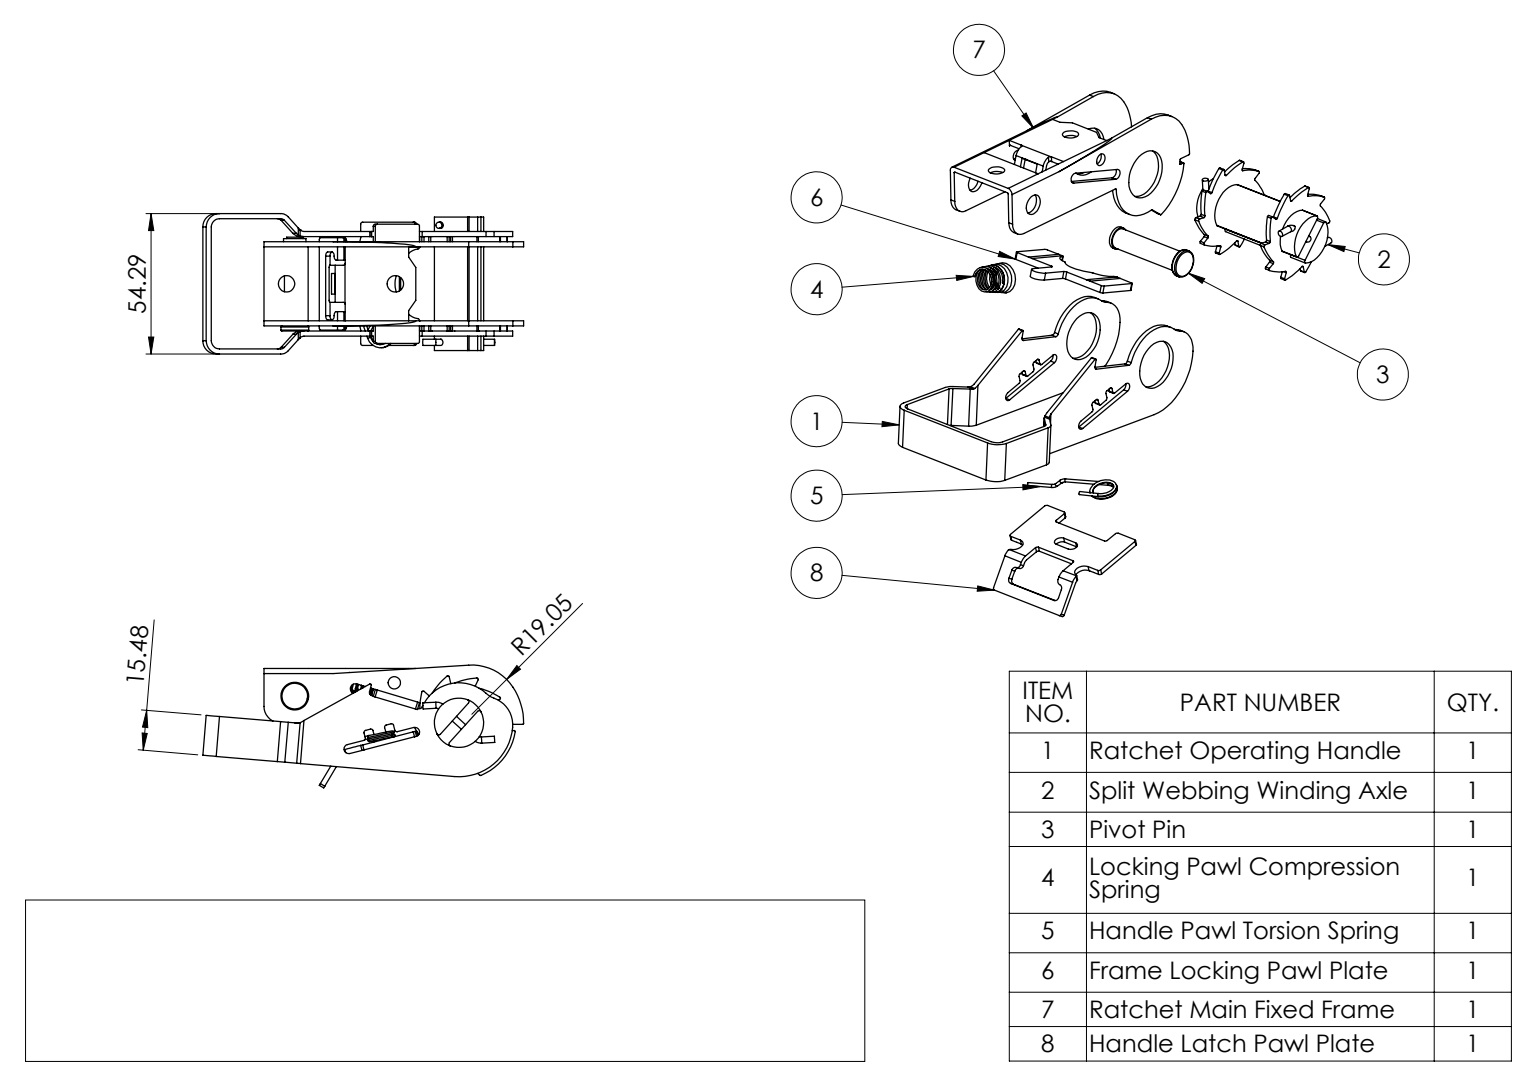
ISO-10303-21;
HEADER;
FILE_DESCRIPTION (('STEP AP214'),
    '1' );
FILE_NAME ('MAS-676',
    '2026-10-09T14:10:49',
    ( '' ),
    ( '' ),
    'SwSTEP 2.0',
    'SolidWorks 2026',
    '' );
FILE_SCHEMA (( 'AUTOMOTIVE_DESIGN' ));
ENDSEC;

DATA;
#1 = VERTEX_POINT ( 'NONE', #18707 ) ;
#2 = CARTESIAN_POINT ( 'NONE',  ( 12.17369753589567871, 10.51393144722840134, 2.800165564711390775 ) ) ;
#3 = CIRCLE ( 'NONE', #8469, 0.5080000000000013394 ) ;
#4 = CARTESIAN_POINT ( 'NONE',  ( 11.85962738539019945, 21.73984789707424170, 3.515838200515787548 ) ) ;
#5 = ORIENTED_EDGE ( 'NONE', *, *, #9450, .F. ) ;
#6 = CARTESIAN_POINT ( 'NONE',  ( 8.350682983910802548, 10.74290543192399028, 2.522985661756687037 ) ) ;
#7 = CARTESIAN_POINT ( 'NONE',  ( 2.865713946637347131, 12.03281576442448042, 5.073952485450168304 ) ) ;
#8 = CARTESIAN_POINT ( 'NONE',  ( -23.01875000000000071, 1.984375000000000000, -3.968750000000000000 ) ) ;
#9 = ADVANCED_FACE ( 'NONE', ( #16944, #16633 ), #1476, .F. ) ;
#10 = CARTESIAN_POINT ( 'NONE',  ( 24.26606285357373594, 2.770822500000000854, -16.92219937337620195 ) ) ;
#11 = CARTESIAN_POINT ( 'NONE',  ( 11.51539948528376733, 12.31998346384714083, 5.480917910381482017 ) ) ;
#12 = VECTOR ( 'NONE', #9469, 1000.000000000000227 ) ;
#13 = VECTOR ( 'NONE', #12201, 1000.000000000000000 ) ;
#14 = CARTESIAN_POINT ( 'NONE',  ( 3.657427262928014677, 14.72322116853433194, 9.063302901626695274 ) ) ;
#15 = CARTESIAN_POINT ( 'NONE',  ( -17.46249999999999858, 1.984375000000000000, 0.000000000000000000 ) ) ;
#16 = CARTESIAN_POINT ( 'NONE',  ( 20.19277141636333894, -1.028702071915735816, -14.77014087419847499 ) ) ;
#17 = CARTESIAN_POINT ( 'NONE',  ( 2.809774020526558225, 19.21875272216368202, 7.448689460942592433 ) ) ;
#18 = CARTESIAN_POINT ( 'NONE',  ( 49.81956284419040060, 0.000000000000000000, 11.98436472153758103 ) ) ;
#19 = CARTESIAN_POINT ( 'NONE',  ( 10.74587282237300023, -3.551474423027108696, -17.13904648846254730 ) ) ;
#20 = STYLED_ITEM ( 'NONE', ( #9424 ), #6575 ) ;
#21 = PLANE ( 'NONE',  #4977 ) ;
#22 = VECTOR ( 'NONE', #6155, 999.9999999999998863 ) ;
#23 = ORIENTED_EDGE ( 'NONE', *, *, #18650, .T. ) ;
#24 = CYLINDRICAL_SURFACE ( 'NONE', #13892, 30.16250000000000142 ) ;
#25 = CARTESIAN_POINT ( 'NONE',  ( 10.71174415246057698, 20.20840087037584709, 6.087647022013951137 ) ) ;
#26 = EDGE_CURVE ( 'NONE', #12400, #1617, #15318, .T. ) ;
#27 = ORIENTED_EDGE ( 'NONE', *, *, #3397, .F. ) ;
#28 = CARTESIAN_POINT ( 'NONE',  ( 12.58269666770059381, 11.55388254762453215, 3.248295542190139606 ) ) ;
#29 = CARTESIAN_POINT ( 'NONE',  ( 53.08681243026497043, 37.69777154208443193, -16.72443647847455850 ) ) ;
#30 = CARTESIAN_POINT ( 'NONE',  ( 16.87573345534896063, 1.342421174834532049, -14.70424319714138583 ) ) ;
#31 = CARTESIAN_POINT ( 'NONE',  ( 6.789087559929837923, 18.21544151669790068, 7.520383359049297667 ) ) ;
#32 = ORIENTED_EDGE ( 'NONE', *, *, #21036, .F. ) ;
#33 = SHAPE_REPRESENTATION_RELATIONSHIP ( 'NONE' , 'NONE' ,  #560, #17207 ) ;
#34 = DIRECTION ( 'NONE',  ( 0.9943660382494290406, 0.000000000000000000, -0.1060008583745199739 ) ) ;
#35 = CARTESIAN_POINT ( 'NONE',  ( -29.36874999999999858, 2.380615000000000148, 8.335010000000000474 ) ) ;
#36 = EDGE_CURVE ( 'NONE', #1582, #17060, #15097, .T. ) ;
#37 = EDGE_CURVE ( 'NONE', #10557, #1153, #11768, .T. ) ;
#38 = ADVANCED_FACE ( 'NONE', ( #13541 ), #20247, .T. ) ;
#39 = CARTESIAN_POINT ( 'NONE',  ( -0.5435003404963313356, 2.373947500000000765, -25.80650133522849998 ) ) ;
#40 = CLOSED_SHELL ( 'NONE', ( #13341, #4807, #5036, #2626, #8435, #8593, #10298, #38, #14436, #19908, #617, #19403, #13246, #15792, #17350, #9101 ) ) ;
#41 = ORIENTED_EDGE ( 'NONE', *, *, #3166, .F. ) ;
#42 = CARTESIAN_POINT ( 'NONE',  ( 9.280550395262261887, 14.88029421051436429, 7.112226467325535317 ) ) ;
#43 = CARTESIAN_POINT ( 'NONE',  ( 11.94459739279681543, 20.94853845629116051, 3.647987758710024675 ) ) ;
#44 = CARTESIAN_POINT ( 'NONE',  ( 3.622293142213341088, 12.24591714145684129, 6.558976304062217544 ) ) ;
#45 = CARTESIAN_POINT ( 'NONE',  ( 6.749462305694075681, 11.05277248166000170, 4.479057920628951805 ) ) ;
#46 = CIRCLE ( 'NONE', #17730, 1.984374999999999112 ) ;
#47 = CARTESIAN_POINT ( 'NONE',  ( 12.03790632155779505, -1.842118199788904453, -16.73074338374886594 ) ) ;
#48 = DIRECTION ( 'NONE',  ( 0.000000000000000000, -1.000000000000000000, 0.000000000000000000 ) ) ;
#49 = ORIENTED_EDGE ( 'NONE', *, *, #10493, .T. ) ;
#50 = CARTESIAN_POINT ( 'NONE',  ( 10.56693948759176571, 19.61111237035978050, 5.589555579635868021 ) ) ;
#51 = CARTESIAN_POINT ( 'NONE',  ( 8.239716553926831111, 21.32987559984598391, 5.052740338774581730 ) ) ;
#52 = EDGE_CURVE ( 'NONE', #9108, #5857, #17721, .T. ) ;
#53 = CARTESIAN_POINT ( 'NONE',  ( 55.27198911326564001, 34.52875999999999834, 2.462719476673013830 ) ) ;
#54 = VECTOR ( 'NONE', #11480, 1000.000000000000000 ) ;
#55 = ORIENTED_EDGE ( 'NONE', *, *, #21504, .F. ) ;
#56 = ORIENTED_EDGE ( 'NONE', *, *, #17494, .T. ) ;
#57 = VECTOR ( 'NONE', #329, 1000.000000000000114 ) ;
#58 = CARTESIAN_POINT ( 'NONE',  ( 47.00675968526287818, 38.88803500000000213, -12.79836188810822328 ) ) ;
#59 = CARTESIAN_POINT ( 'NONE',  ( 11.16210623263107848, 18.34813493204594081, -4.029110776031238572 ) ) ;
#61 = CARTESIAN_POINT ( 'NONE',  ( 14.43917063414567536, -6.754812500000002551, 2.343183994106907697 ) ) ;
#60 = CARTESIAN_POINT ( 'NONE',  ( 2.165347194003833575, 20.74767509450332170, 6.678208812454825782 ) ) ;
#62 = ORIENTED_EDGE ( 'NONE', *, *, #7822, .T. ) ;
#63 = CARTESIAN_POINT ( 'NONE',  ( 6.018011364848629974, 21.34202296141599930, 4.812272833256288074 ) ) ;
#64 = VECTOR ( 'NONE', #8370, 1000.000000000000000 ) ;
#65 = DIRECTION ( 'NONE',  ( 0.000000000000000000, 0.000000000000000000, -1.000000000000000000 ) ) ;
#66 = ORIENTED_EDGE ( 'NONE', *, *, #20020, .T. ) ;
#67 = AXIS2_PLACEMENT_3D ( 'NONE', #9052, #15829, #7402 ) ;
#68 = EDGE_CURVE ( 'NONE', #10096, #18019, #3909, .T. ) ;
#69 = DIRECTION ( 'NONE',  ( -0.000000000000000000, -1.000000000000000000, 0.000000000000000000 ) ) ;
#70 = ORIENTED_EDGE ( 'NONE', *, *, #12967, .F. ) ;
#71 = AXIS2_PLACEMENT_3D ( 'NONE', #14766, #21802, #18271 ) ;
#72 = CYLINDRICAL_SURFACE ( 'NONE', #449, 30.16250000000000142 ) ;
#73 = DIRECTION ( 'NONE',  ( 0.000000000000000000, -1.000000000000000000, 0.000000000000000000 ) ) ;
#74 = PLANE ( 'NONE',  #18206 ) ;
#75 = CARTESIAN_POINT ( 'NONE',  ( 2.895144775783714763, 20.91827869092655945, 2.067392077668602113 ) ) ;
#76 = AXIS2_PLACEMENT_3D ( 'NONE', #2154, #5245, #12004 ) ;
#77 = CYLINDRICAL_SURFACE ( 'NONE', #10849, 0.5080000000000005622 ) ;
#78 = VECTOR ( 'NONE', #17853, 1000.000000000000227 ) ;
#79 = ORIENTED_EDGE ( 'NONE', *, *, #17597, .T. ) ;
#80 = DIRECTION ( 'NONE',  ( 0.000000000000000000, 1.000000000000000000, 0.000000000000000000 ) ) ;
#81 = LINE ( 'NONE', #19981, #4674 ) ;
#82 = CARTESIAN_POINT ( 'NONE',  ( 29.01020070778135818, -3.968114999999999615, -13.85841188422236492 ) ) ;
#83 = EDGE_CURVE ( 'NONE', #6123, #21755, #12204, .T. ) ;
#84 = DIRECTION ( 'NONE',  ( 0.000000000000000000, 1.000000000000000000, 0.000000000000000000 ) ) ;
#86 = CARTESIAN_POINT ( 'NONE',  ( 19.20082524333561125, -5.215953177437151034, -14.22689379871408022 ) ) ;
#85 = CARTESIAN_POINT ( 'NONE',  ( -47.86112874365709047, 43.41875999999999891, -23.29368419115692035 ) ) ;
#87 = ORIENTED_EDGE ( 'NONE', *, *, #3995, .F. ) ;
#88 = ADVANCED_FACE ( 'NONE', ( #14317 ), #12096, .F. ) ;
#89 = ORIENTED_EDGE ( 'NONE', *, *, #190, .T. ) ;
#90 = CARTESIAN_POINT ( 'NONE',  ( 9.174791387338732562, 15.41930233576164433, -2.840203025228832612 ) ) ;
#92 = CARTESIAN_POINT ( 'NONE',  ( 39.27728671717661513, 34.52875999999999834, -23.95520057284206672 ) ) ;
#91 = CARTESIAN_POINT ( 'NONE',  ( 2.493085962414791190, 11.21420404894608147, 3.435105624136618907 ) ) ;
#93 = VERTEX_POINT ( 'NONE', #19156 ) ;
#94 = AXIS2_PLACEMENT_3D ( 'NONE', #5064, #16687, #13274 ) ;
#95 = ORIENTED_EDGE ( 'NONE', *, *, #5447, .T. ) ;
#96 = DIRECTION ( 'NONE',  ( 0.000000000000000000, 1.000000000000000000, 0.000000000000000000 ) ) ;
#97 = VERTEX_POINT ( 'NONE', #18926 ) ;
#98 = CARTESIAN_POINT ( 'NONE',  ( 9.266976129945037499, 14.72489524569131092, 6.957161557103688665 ) ) ;
#99 = VECTOR ( 'NONE', #5317, 1000.000000000000114 ) ;
#100 = CARTESIAN_POINT ( 'NONE',  ( 3.378324179703998453, 14.02502511948407715, 7.785346146968057823 ) ) ;
#101 = DIRECTION ( 'NONE',  ( -0.6702301885068630005, 0.000000000000000000, -0.7421532822901580895 ) ) ;
#102 = VECTOR ( 'NONE', #21181, 1000.000000000000114 ) ;
#103 = DIRECTION ( 'NONE',  ( -0.2035550397114870846, 0.000000000000000000, -0.9790635044817342925 ) ) ;
#104 = CYLINDRICAL_SURFACE ( 'NONE', #7585, 0.3962400000000010358 ) ;
#105 = CARTESIAN_POINT ( 'NONE',  ( 0.7283536316373762087, 20.30898886747102594, 1.952961586103617142 ) ) ;
#106 = FACE_OUTER_BOUND ( 'NONE', #16454, .T. ) ;
#107 = VERTEX_POINT ( 'NONE', #482 ) ;
#108 = CARTESIAN_POINT ( 'NONE',  ( 6.774501940737490457, 19.51815128457440451, 6.453198523737214920 ) ) ;
#109 = CARTESIAN_POINT ( 'NONE',  ( 46.03750000000000142, 0.000000000000000000, -10.31874999999999964 ) ) ;
#110 = CARTESIAN_POINT ( 'NONE',  ( 53.77834614425744064, -5.598900522968899729, -15.87027249378376936 ) ) ;
#111 = DIRECTION ( 'NONE',  ( 0.2490110332224850509, 0.000000000000000000, -0.9685006480810792739 ) ) ;
#112 = CYLINDRICAL_SURFACE ( 'NONE', #2785, 0.5079999999999976756 ) ;
#113 = EDGE_LOOP ( 'NONE', ( #12441, #427, #14936, #388, #14608 ) ) ;
#114 = EDGE_CURVE ( 'NONE', #97, #11029, #5668, .T. ) ;
#115 = CARTESIAN_POINT ( 'NONE',  ( 13.04354795994631111, 16.76121402582646880, 7.282986886760092204 ) ) ;
#116 = AXIS2_PLACEMENT_3D ( 'NONE', #2669, #1515, #18221 ) ;
#117 = CARTESIAN_POINT ( 'NONE',  ( 36.51250000000000284, 30.56064500000000095, -10.31875000000000142 ) ) ;
#118 = CARTESIAN_POINT ( 'NONE',  ( 13.35587560995692868, 16.38622677847037679, 7.171674097283092131 ) ) ;
#119 = VERTEX_POINT ( 'NONE', #18820 ) ;
#120 = EDGE_LOOP ( 'NONE', ( #10937, #5548, #3135, #2897 ) ) ;
#121 = CARTESIAN_POINT ( 'NONE',  ( 8.292815045765784987, 10.74474575179219116, 2.280097550029496656 ) ) ;
#122 = CARTESIAN_POINT ( 'NONE',  ( 0.8394066731220519717, 19.67029402086490109, 2.252889122871652106 ) ) ;
#123 = DIRECTION ( 'NONE',  ( 0.2868778675745011220, 0.000000000000000000, 0.9579671649362034858 ) ) ;
#124 = CARTESIAN_POINT ( 'NONE',  ( 1.780815508985763129, 20.40739888885963182, 4.751999544564226241 ) ) ;
#125 = PLANE ( 'NONE',  #13958 ) ;
#126 = CARTESIAN_POINT ( 'NONE',  ( 14.41880979295608078, 20.66289627653780059, 3.789204515037973398 ) ) ;
#127 = CARTESIAN_POINT ( 'NONE',  ( 5.346755153171518948, 14.26008107018554760, 7.537986371638543126 ) ) ;
#128 = VECTOR ( 'NONE', #842, 1000.000000000000000 ) ;
#129 = CARTESIAN_POINT ( 'NONE',  ( 0.1976838887606784945, 19.02276410538376084, 0.6665157320697154830 ) ) ;
#130 = CARTESIAN_POINT ( 'NONE',  ( 13.67756757867809725, 20.23395749999999893, 2.571257636385987144 ) ) ;
#131 = CARTESIAN_POINT ( 'NONE',  ( 19.71883509336728224, 0.07040483093252521141, -14.88702419437599112 ) ) ;
#132 = CARTESIAN_POINT ( 'NONE',  ( -0.8299773975634847645, 19.84689652320655995, 3.579766241068111476 ) ) ;
#133 = DIRECTION ( 'NONE',  ( -0.9980811434661737147, 0.000000000000000000, -0.06191955310929838502 ) ) ;
#134 = CARTESIAN_POINT ( 'NONE',  ( 18.64212857235120069, -7.698692359554816456, -15.50269025218566021 ) ) ;
#135 = VECTOR ( 'NONE', #21119, 1000.000000000000000 ) ;
#136 = CARTESIAN_POINT ( 'NONE',  ( 20.56513292926062775, -14.84248999999999974, -10.49765270116350280 ) ) ;
#137 = EDGE_CURVE ( 'NONE', #6597, #20373, #21240, .T. ) ;
#138 = VERTEX_POINT ( 'NONE', #587 ) ;
#139 = DIRECTION ( 'NONE',  ( 0.05085730733808393328, 0.000000000000000000, -0.9987059298363656357 ) ) ;
#140 = CARTESIAN_POINT ( 'NONE',  ( 9.883496637816898911, 21.64168280960603141, 3.868047802342164498 ) ) ;
#141 = DIRECTION ( 'NONE',  ( 0.000000000000000000, 1.000000000000000000, 0.000000000000000000 ) ) ;
#142 = ORIENTED_EDGE ( 'NONE', *, *, #11602, .F. ) ;
#143 = CARTESIAN_POINT ( 'NONE',  ( 12.42291455053379856, 11.33033927736581248, 2.552232267275179822 ) ) ;
#144 = LINE ( 'NONE', #10317, #14114 ) ;
#146 = LINE ( 'NONE', #8543, #21177 ) ;
#145 = CARTESIAN_POINT ( 'NONE',  ( -0.7347962684923032839, 20.04712316396406280, 3.997874094937027944 ) ) ;
#147 = VECTOR ( 'NONE', #5994, 1000.000000000000114 ) ;
#148 = ORIENTED_EDGE ( 'NONE', *, *, #13327, .T. ) ;
#149 = EDGE_CURVE ( 'NONE', #1153, #19768, #10533, .T. ) ;
#150 = DIRECTION ( 'NONE',  ( 0.000000000000000000, -1.000000000000000000, 0.000000000000000000 ) ) ;
#151 = CARTESIAN_POINT ( 'NONE',  ( 4.296253888929676634, 19.19961258863813214, 0.3083300652943509745 ) ) ;
#152 = CARTESIAN_POINT ( 'NONE',  ( 6.396056618077795797, 11.71523274630726164, 2.847703469759983008 ) ) ;
#153 = VECTOR ( 'NONE', #12221, 1000.000000000000114 ) ;
#154 = ORIENTED_EDGE ( 'NONE', *, *, #19245, .T. ) ;
#155 = CARTESIAN_POINT ( 'NONE',  ( 8.179867684019033192, 11.48837196139402295, 1.858590186261403598 ) ) ;
#156 = CARTESIAN_POINT ( 'NONE',  ( 3.477066233666421979, 20.55600749251701842, 3.648995514013453789 ) ) ;
#157 = EDGE_CURVE ( 'NONE', #13662, #8452, #17280, .T. ) ;
#158 = CARTESIAN_POINT ( 'NONE',  ( 13.15265190013183449, 16.70050942663215210, 6.498420246545746792 ) ) ;
#159 = CARTESIAN_POINT ( 'NONE',  ( 3.286495487773421598, 20.56225727104456169, 1.886831981940775949 ) ) ;
#160 = CARTESIAN_POINT ( 'NONE',  ( 7.189655306835470938, 16.38024503317697622, -2.993817834679030288 ) ) ;
#161 = VECTOR ( 'NONE', #4886, 1000.000000000000227 ) ;
#162 = LINE ( 'NONE', #18727, #15361 ) ;
#163 = CARTESIAN_POINT ( 'NONE',  ( 13.41487274969213317, -6.317043706895210775, -16.60971403326354334 ) ) ;
#164 = CARTESIAN_POINT ( 'NONE',  ( 14.93145837000203358, 15.36419388438619826, -20.01065317369261365 ) ) ;
#165 = EDGE_CURVE ( 'NONE', #19859, #2625, #8173, .T. ) ;
#166 = ORIENTED_EDGE ( 'NONE', *, *, #3462, .T. ) ;
#167 = ADVANCED_FACE ( 'NONE', ( #2245 ), #15977, .T. ) ;
#168 = CARTESIAN_POINT ( 'NONE',  ( 11.06414373101206117, 17.47476261052015190, 6.688118229093674039 ) ) ;
#169 = CARTESIAN_POINT ( 'NONE',  ( 7.463855498632248953, 18.37204556237463393, -2.667043638653753490 ) ) ;
#170 = VECTOR ( 'NONE', #3329, 1000.000000000000000 ) ;
#171 = VERTEX_POINT ( 'NONE', #19036 ) ;
#172 = DIRECTION ( 'NONE',  ( 0.000000000000000000, 1.000000000000000000, 0.000000000000000000 ) ) ;
#173 = LINE ( 'NONE', #16974, #9614 ) ;
#175 = DIRECTION ( 'NONE',  ( -0.1060008583745224581, 0.000000000000000000, -0.9943660382494288186 ) ) ;
#174 = CARTESIAN_POINT ( 'NONE',  ( 3.353433880231968534, 14.74976095948969679, 9.067427483657878540 ) ) ;
#176 = ORIENTED_EDGE ( 'NONE', *, *, #8308, .T. ) ;
#177 = CARTESIAN_POINT ( 'NONE',  ( 7.475884085846502103, 16.82090011607979463, 8.373859609186036224 ) ) ;
#178 = ORIENTED_EDGE ( 'NONE', *, *, #11385, .F. ) ;
#179 = DIRECTION ( 'NONE',  ( -0.2490110332224836354, 0.000000000000000000, 0.9685006480810794960 ) ) ;
#180 = VERTEX_POINT ( 'NONE', #9193 ) ;
#181 = CARTESIAN_POINT ( 'NONE',  ( 1.895584402099029120, 14.60931841795548536, 0.4380894700145442355 ) ) ;
#182 = ADVANCED_FACE ( 'NONE', ( #3687 ), #8750, .T. ) ;
#183 = AXIS2_PLACEMENT_3D ( 'NONE', #21265, #19500, #6119 ) ;
#184 = CARTESIAN_POINT ( 'NONE',  ( 14.93145837000203358, 15.36419388438619826, -20.01065317369261365 ) ) ;
#185 = LINE ( 'NONE', #17106, #9522 ) ;
#186 = CARTESIAN_POINT ( 'NONE',  ( -13.57684171658811678, 32.54247999999999763, -0.8078590638549644209 ) ) ;
#187 = CARTESIAN_POINT ( 'NONE',  ( 5.129543141202642431, 19.14094820344656256, 7.993442615763653336 ) ) ;
#188 = CYLINDRICAL_SURFACE ( 'NONE', #17566, 0.5080000000000007843 ) ;
#189 = ORIENTED_EDGE ( 'NONE', *, *, #13845, .T. ) ;
#190 = EDGE_CURVE ( 'NONE', #7494, #14487, #7555, .T. ) ;
#191 = CARTESIAN_POINT ( 'NONE',  ( 53.25483508941461963, 42.06303499999999929, -5.879799058943532941 ) ) ;
#192 = CARTESIAN_POINT ( 'NONE',  ( 1.416441012474747074, 34.09397655050049991, -20.74814719358345627 ) ) ;
#193 =( NAMED_UNIT ( * ) PLANE_ANGLE_UNIT ( ) SI_UNIT ( $, .RADIAN. ) );
#194 = CARTESIAN_POINT ( 'NONE',  ( 13.97919557092905407, 2.287850299137407006, -16.10306415954642389 ) ) ;
#196 = CARTESIAN_POINT ( 'NONE',  ( 19.79930818132203285, -2.883721276782408083, -14.18765533889165553 ) ) ;
#195 = DIRECTION ( 'NONE',  ( 0.000000000000000000, 1.000000000000000000, 0.000000000000000000 ) ) ;
#197 = ORIENTED_EDGE ( 'NONE', *, *, #8367, .F. ) ;
#198 = ORIENTED_EDGE ( 'NONE', *, *, #7883, .F. ) ;
#199 = CARTESIAN_POINT ( 'NONE',  ( 12.51949563173172741, 11.87357545845056173, 4.349419763020000218 ) ) ;
#201 = LINE ( 'NONE', #6943, #11370 ) ;
#200 = CARTESIAN_POINT ( 'NONE',  ( 6.311431466362975584, 21.18174881316136293, 5.533192182388949831 ) ) ;
#202 = ORIENTED_EDGE ( 'NONE', *, *, #14570, .F. ) ;
#203 = EDGE_CURVE ( 'NONE', #6199, #19184, #15619, .T. ) ;
#204 = ORIENTED_EDGE ( 'NONE', *, *, #16141, .T. ) ;
#205 = CARTESIAN_POINT ( 'NONE',  ( 29.36874999999999858, 0.000000000000000000, 10.71562499999999929 ) ) ;
#206 = EDGE_LOOP ( 'NONE', ( #18423, #5151, #18532, #223 ) ) ;
#207 = CARTESIAN_POINT ( 'NONE',  ( 7.493187710091532061, 16.56948303458045402, -2.124950967123346857 ) ) ;
#208 = DIRECTION ( 'NONE',  ( 0.9767031480033349089, 0.000000000000000000, -0.2145948757085681391 ) ) ;
#209 = ORIENTED_EDGE ( 'NONE', *, *, #16573, .T. ) ;
#210 = EDGE_CURVE ( 'NONE', #9895, #180, #14097, .T. ) ;
#211 = ADVANCED_FACE ( 'NONE', ( #17509 ), #9084, .T. ) ;
#212 = EDGE_CURVE ( 'NONE', #18633, #13378, #14563, .T. ) ;
#213 = DIRECTION ( 'NONE',  ( 0.2064631973582987667, 0.000000000000000000, -0.9784543669157944601 ) ) ;
#214 = DIRECTION ( 'NONE',  ( 0.000000000000000000, 1.000000000000000000, 0.000000000000000000 ) ) ;
#215 = CARTESIAN_POINT ( 'NONE',  ( 4.520836821130160388, 5.548947500000001476, -5.476444653012091379 ) ) ;
#216 = CARTESIAN_POINT ( 'NONE',  ( 19.79515554403045741, -1.983739999999999393, -10.69562145279641996 ) ) ;
#217 = CARTESIAN_POINT ( 'NONE',  ( -0.001022716578500358631, 17.78166323453216791, 0.2331896389956350235 ) ) ;
#218 = VERTEX_POINT ( 'NONE', #12980 ) ;
#219 = CARTESIAN_POINT ( 'NONE',  ( 7.380557675095882786, 16.58762552368920851, 7.687920665816121435 ) ) ;
#220 = DIRECTION ( 'NONE',  ( 0.000000000000000000, -1.000000000000000000, 0.000000000000000000 ) ) ;
#221 = CYLINDRICAL_SURFACE ( 'NONE', #1464, 0.5079999999999963434 ) ;
#222 = PLANE ( 'NONE',  #19482 ) ;
#223 = ORIENTED_EDGE ( 'NONE', *, *, #6828, .F. ) ;
#224 = CARTESIAN_POINT ( 'NONE',  ( 13.93482735099323833, 21.64660035503122160, 3.717575555280015376 ) ) ;
#225 = CARTESIAN_POINT ( 'NONE',  ( 64.14292646034530776, 0.000000000000000000, -12.24881465648521939 ) ) ;
#226 = CARTESIAN_POINT ( 'NONE',  ( 13.26836735398159028, 17.42901524731493268, 7.078061169219369120 ) ) ;
#227 = VERTEX_POINT ( 'NONE', #17942 ) ;
#228 = ORIENTED_EDGE ( 'NONE', *, *, #15345, .F. ) ;
#229 = CARTESIAN_POINT ( 'NONE',  ( 38.18512253410862201, -6.356984999999999886, -4.927479914652648674 ) ) ;
#230 = CARTESIAN_POINT ( 'NONE',  ( 9.479476315004470521, 15.99709907451843094, 7.980467261906161625 ) ) ;
#231 = CARTESIAN_POINT ( 'NONE',  ( 0.4810215415031842134, 12.38241104890028232, 3.423352113816969577 ) ) ;
#232 = CARTESIAN_POINT ( 'NONE',  ( 9.410620405120566190, 30.63641399982339308, -22.17591973292933361 ) ) ;
#233 = CARTESIAN_POINT ( 'NONE',  ( 5.697655638014817114, 17.11702998724009461, -1.340185189716478931 ) ) ;
#234 = CARTESIAN_POINT ( 'NONE',  ( 7.228545246289955095, 16.94088807395186791, 7.597636453550198787 ) ) ;
#235 = CARTESIAN_POINT ( 'NONE',  ( 1.159471316600563018, 20.10462493015178964, 3.144633053345586404 ) ) ;
#236 = CARTESIAN_POINT ( 'NONE',  ( -24.21104940531825633, 39.44874000000000080, -25.29232732678598339 ) ) ;
#237 = EDGE_CURVE ( 'NONE', #10280, #1619, #6209, .T. ) ;
#238 = CARTESIAN_POINT ( 'NONE',  ( 54.11611804786240043, 30.56064500000000095, -30.58983753981140197 ) ) ;
#239 = AXIS2_PLACEMENT_3D ( 'NONE', #18075, #4699, #2934 ) ;
#240 = CARTESIAN_POINT ( 'NONE',  ( 7.753680531148133603, 16.37218494104095967, -2.740645328831583960 ) ) ;
#241 = CARTESIAN_POINT ( 'NONE',  ( 5.362875270629205104, 14.52669407825994696, 7.666357001590486497 ) ) ;
#242 = CARTESIAN_POINT ( 'NONE',  ( 1.227981727922097921, 21.11436061630988092, 3.317903474119387575 ) ) ;
#243 = DIRECTION ( 'NONE',  ( -0.1831666983863990128, 0.000000000000000000, 0.9830818687180767901 ) ) ;
#244 = DIRECTION ( 'NONE',  ( 0.8609107660235850723, 0.000000000000000000, -0.5087559856598092844 ) ) ;
#245 = CARTESIAN_POINT ( 'NONE',  ( 1.820039393668895888, 20.48353144049298180, 4.932753874264384386 ) ) ;
#246 = CYLINDRICAL_SURFACE ( 'NONE', #5483, 3.970019999999997662 ) ;
#247 = CARTESIAN_POINT ( 'NONE',  ( 11.07281055964317495, -1.101114635511414530, -16.96369225983369944 ) ) ;
#248 = CARTESIAN_POINT ( 'NONE',  ( 53.46798503507454825, 34.52875999999999834, 6.304111036318381878 ) ) ;
#249 = CARTESIAN_POINT ( 'NONE',  ( 9.544203190417185567, 21.84156436469462292, 2.933652179873399213 ) ) ;
#250 = FACE_OUTER_BOUND ( 'NONE', #17892, .T. ) ;
#251 = ORIENTED_EDGE ( 'NONE', *, *, #17974, .F. ) ;
#252 = CARTESIAN_POINT ( 'NONE',  ( 11.27018246201781260, 13.25626094221269646, -2.577908581355527140 ) ) ;
#253 = AXIS2_PLACEMENT_3D ( 'NONE', #9461, #16230, #5826 ) ;
#254 = DIRECTION ( 'NONE',  ( -0.000000000000000000, -1.000000000000000000, 0.000000000000000000 ) ) ;
#255 = PLANE ( 'NONE',  #7057 ) ;
#256 = ORIENTED_EDGE ( 'NONE', *, *, #13831, .T. ) ;
#257 = APPLICATION_PROTOCOL_DEFINITION ( 'draft international standard', 'automotive_design', 1998, #9318 ) ;
#258 = CARTESIAN_POINT ( 'NONE',  ( -13.87747867115857936, -3.968114999999999615, -9.458632424640695646 ) ) ;
#259 = LINE ( 'NONE', #5449, #10897 ) ;
#260 = CARTESIAN_POINT ( 'NONE',  ( 6.053719233771420960, 11.12068933878565247, 2.906810406936975344 ) ) ;
#261 = EDGE_CURVE ( 'NONE', #11029, #831, #7657, .T. ) ;
#262 = CARTESIAN_POINT ( 'NONE',  ( 18.00364882752649720, -8.167742914975729462, -14.89596189428242567 ) ) ;
#263 = ORIENTED_EDGE ( 'NONE', *, *, #13066, .F. ) ;
#264 = CARTESIAN_POINT ( 'NONE',  ( 9.225191506351318793, 16.57983669178404895, 7.321902877288878564 ) ) ;
#265 = CARTESIAN_POINT ( 'NONE',  ( 6.962953135734946564, 20.81446147317312168, 1.610669861356619936 ) ) ;
#266 = CARTESIAN_POINT ( 'NONE',  ( 5.021296906522759507, 20.20829226350481989, 6.496222906105421302 ) ) ;
#267 = CARTESIAN_POINT ( 'NONE',  ( 9.106845709993205418, 13.32481467742428016, -2.904340219645574983 ) ) ;
#268 = CIRCLE ( 'NONE', #3100, 1.190624999999997824 ) ;
#269 = DIRECTION ( 'NONE',  ( -0.9685006480810792739, 0.000000000000000000, -0.2490110332224846346 ) ) ;
#270 = CARTESIAN_POINT ( 'NONE',  ( 14.14748371971443675, 0.7006734101483724775, -16.02524869538980212 ) ) ;
#271 = DIRECTION ( 'NONE',  ( 0.000000000000000000, 1.000000000000000000, 0.000000000000000000 ) ) ;
#272 = EDGE_CURVE ( 'NONE', #13945, #11658, #11090, .T. ) ;
#273 = ORIENTED_EDGE ( 'NONE', *, *, #1147, .T. ) ;
#274 = CARTESIAN_POINT ( 'NONE',  ( 11.18299850411455232, 14.10173808182719135, 6.301220783482575527 ) ) ;
#275 = CARTESIAN_POINT ( 'NONE',  ( 9.073444559871269632, 11.49988781216720213, 5.501919269197937723 ) ) ;
#276 = EDGE_LOOP ( 'NONE', ( #21374, #11121, #4887, #17818 ) ) ;
#277 = DIRECTION ( 'NONE',  ( 0.9964481331860212121, 0.000000000000000000, -0.08420877549337300871 ) ) ;
#278 = DIRECTION ( 'NONE',  ( 0.000000000000000000, -1.000000000000000000, 0.000000000000000000 ) ) ;
#280 = DIRECTION ( 'NONE',  ( 0.000000000000000000, 1.000000000000000000, 0.000000000000000000 ) ) ;
#279 = CARTESIAN_POINT ( 'NONE',  ( 3.327436967205598339, 17.33544538521946876, -1.277308115045836523 ) ) ;
#281 = ORIENTED_EDGE ( 'NONE', *, *, #11678, .T. ) ;
#282 = CARTESIAN_POINT ( 'NONE',  ( 6.938136749357236788, 11.33047045554270227, 5.170081444403209048 ) ) ;
#283 = DIRECTION ( 'NONE',  ( 0.7334850928793773539, -0.6768732144311023768, -0.06198604769976986950 ) ) ;
#284 = VECTOR ( 'NONE', #21016, 1000.000000000000000 ) ;
#285 = ORIENTED_EDGE ( 'NONE', *, *, #4081, .F. ) ;
#286 = EDGE_CURVE ( 'NONE', #20627, #1656, #19688, .T. ) ;
#287 = CARTESIAN_POINT ( 'NONE',  ( 18.07371581377308800, 36.51313500000000545, -11.95909761906105473 ) ) ;
#288 = VERTEX_POINT ( 'NONE', #14647 ) ;
#289 = EDGE_CURVE ( 'NONE', #5674, #3944, #16188, .T. ) ;
#290 = CARTESIAN_POINT ( 'NONE',  ( 6.016625000000000334, 1.984375000000000000, 2.794000000000000039 ) ) ;
#291 = CARTESIAN_POINT ( 'NONE',  ( -29.36874999999999858, 9.129395000000000593, 0.000000000000000000 ) ) ;
#292 = CARTESIAN_POINT ( 'NONE',  ( 29.98909767165928386, 30.50833916023545811, -5.214162619065493054 ) ) ;
#293 = CARTESIAN_POINT ( 'NONE',  ( 49.41195815393805901, -1.983739999999997838, -1.411525001868561224 ) ) ;
#294 = CARTESIAN_POINT ( 'NONE',  ( 4.339045286082956032, 20.93870084934459186, 5.966996860266638336 ) ) ;
#295 = CARTESIAN_POINT ( 'NONE',  ( 18.65312499999999929, 0.000000000000000000, 5.159374999999999822 ) ) ;
#296 = CIRCLE ( 'NONE', #18309, 1.983739999999999393 ) ;
#297 = ORIENTED_EDGE ( 'NONE', *, *, #14274, .F. ) ;
#298 = DIRECTION ( 'NONE',  ( -0.4857267349359786768, 0.000000000000000000, 0.8741107132214052111 ) ) ;
#299 = DIRECTION ( 'NONE',  ( -0.5222415575336509797, 0.000000000000000000, -0.8527976052879290281 ) ) ;
#300 = DIRECTION ( 'NONE',  ( -0.5087559856598092844, -0.000000000000000000, -0.8609107660235850723 ) ) ;
#301 = DIRECTION ( 'NONE',  ( 0.000000000000000000, 1.000000000000000000, 0.000000000000000000 ) ) ;
#303 = CARTESIAN_POINT ( 'NONE',  ( 12.81960190910725750, -6.042093227902952002, -15.51352245845575695 ) ) ;
#302 = CARTESIAN_POINT ( 'NONE',  ( 32.18388890846549799, 32.54502000000000095, 1.507793899792891468 ) ) ;
#304 = VERTEX_POINT ( 'NONE', #16295 ) ;
#305 = EDGE_LOOP ( 'NONE', ( #11333, #11552, #10599, #2404 ) ) ;
#306 = CARTESIAN_POINT ( 'NONE',  ( 11.70396778136748850, 11.04557676861940152, 0.8370681489755618099 ) ) ;
#308 = FACE_OUTER_BOUND ( 'NONE', #12169, .T. ) ;
#307 = CARTESIAN_POINT ( 'NONE',  ( 3.459298138910898768, 21.44911200421750053, 3.505279687176134473 ) ) ;
#309 = ORIENTED_EDGE ( 'NONE', *, *, #592, .F. ) ;
#310 = CARTESIAN_POINT ( 'NONE',  ( 5.577942838035520268, 14.33718092923608189, 8.413711891740923932 ) ) ;
#311 = EDGE_CURVE ( 'NONE', #1101, #20045, #18407, .T. ) ;
#312 = ORIENTED_EDGE ( 'NONE', *, *, #165, .T. ) ;
#313 = DIRECTION ( 'NONE',  ( 0.000000000000000000, -1.000000000000000000, 0.000000000000000000 ) ) ;
#314 = ORIENTED_EDGE ( 'NONE', *, *, #1169, .F. ) ;
#315 = CARTESIAN_POINT ( 'NONE',  ( 7.680790805331456639, 18.03565907245706157, -1.845473237927973909 ) ) ;
#316 = EDGE_CURVE ( 'NONE', #18861, #19124, #21090, .T. ) ;
#317 = AXIS2_PLACEMENT_3D ( 'NONE', #448, #20660, #3437 ) ;
#318 = ORIENTED_EDGE ( 'NONE', *, *, #7660, .F. ) ;
#319 = EDGE_CURVE ( 'NONE', #2537, #9809, #10285, .T. ) ;
#320 = CARTESIAN_POINT ( 'NONE',  ( 3.353557634575417445, 13.78425396933717550, 7.627037753281808108 ) ) ;
#321 = DIRECTION ( 'NONE',  ( 0.000000000000000000, 1.000000000000000000, 0.000000000000000000 ) ) ;
#322 = CARTESIAN_POINT ( 'NONE',  ( 1.954387715434429795, -42.42568807200000691, 6.745605000000000295 ) ) ;
#323 = CARTESIAN_POINT ( 'NONE',  ( 67.40134256979101224, 0.000000000000000000, -13.70358117861468017 ) ) ;
#324 = CARTESIAN_POINT ( 'NONE',  ( 1.894691563267759227, 21.17677690942452173, 5.065541174868540608 ) ) ;
#325 = CARTESIAN_POINT ( 'NONE',  ( 39.16413618835606769, 37.11476346399999926, -24.45043885672975392 ) ) ;
#326 = ORIENTED_EDGE ( 'NONE', *, *, #979, .T. ) ;
#327 = CARTESIAN_POINT ( 'NONE',  ( 3.920009176498074233, 17.18772947144893948, -0.7115550442440029544 ) ) ;
#328 = DIRECTION ( 'NONE',  ( -0.2490110332224850509, 0.000000000000000000, 0.9685006480810792739 ) ) ;
#329 = DIRECTION ( 'NONE',  ( -0.9685006480810792739, 0.000000000000000000, -0.2490110332224846346 ) ) ;
#330 = DIRECTION ( 'NONE',  ( 0.000000000000000000, 1.000000000000000000, 0.000000000000000000 ) ) ;
#331 = ORIENTED_EDGE ( 'NONE', *, *, #18672, .F. ) ;
#332 = CARTESIAN_POINT ( 'NONE',  ( 11.14915617881719889, 15.67423727725497606, 7.664175941428390537 ) ) ;
#333 = CARTESIAN_POINT ( 'NONE',  ( 6.380166963026771221, 10.92343582149830183, 2.794643371853744007 ) ) ;
#334 = CARTESIAN_POINT ( 'NONE',  ( 13.12613710073441986, 18.43276909965920396, 6.801715849308650697 ) ) ;
#335 = ORIENTED_EDGE ( 'NONE', *, *, #14252, .F. ) ;
#336 = EDGE_CURVE ( 'NONE', #2732, #10479, #8823, .T. ) ;
#337 = VERTEX_POINT ( 'NONE', #7187 ) ;
#338 = CARTESIAN_POINT ( 'NONE',  ( -15.39353573898878658, -2.254660308866960339, -10.30107656633069979 ) ) ;
#339 = EDGE_CURVE ( 'NONE', #11891, #20381, #4666, .T. ) ;
#340 = CARTESIAN_POINT ( 'NONE',  ( 9.473890731828024769, 14.30658367118552654, 7.614261666668934225 ) ) ;
#341 = CARTESIAN_POINT ( 'NONE',  ( 1.873443166787216674, 20.48353144049298180, 4.916761300496329312 ) ) ;
#342 = DIRECTION ( 'NONE',  ( -0.6496772031432439531, 0.000000000000000000, 0.7602101891687401691 ) ) ;
#343 = AXIS2_PLACEMENT_3D ( 'NONE', #9406, #14736, #16073 ) ;
#344 = CARTESIAN_POINT ( 'NONE',  ( 5.621998597895612626, 14.20914477843347257, -0.8778548432169819282 ) ) ;
#345 = DIRECTION ( 'NONE',  ( 0.000000000000000000, 1.000000000000000000, 0.000000000000000000 ) ) ;
#346 = VECTOR ( 'NONE', #19998, 1000.000000000000114 ) ;
#347 = CARTESIAN_POINT ( 'NONE',  ( 12.61840913414979148, 21.24843477279145887, -1.488277761717505143 ) ) ;
#348 = CARTESIAN_POINT ( 'NONE',  ( 38.84235393761607469, -5.162860800152350826, -4.075279525839791361 ) ) ;
#349 = CARTESIAN_POINT ( 'NONE',  ( 0.2609373283441706048, 20.95713891276306029, 6.401234835325384509 ) ) ;
#350 = CARTESIAN_POINT ( 'NONE',  ( 0.04756687825572484402, 20.98775885821133969, 5.773728306871808158 ) ) ;
#351 = CARTESIAN_POINT ( 'NONE',  ( 20.07318776485353240, -0.6525838462317746780, -14.80377008654006055 ) ) ;
#352 = AXIS2_PLACEMENT_3D ( 'NONE', #14843, #6560, #1786 ) ;
#353 = DIRECTION ( 'NONE',  ( 0.000000000000000000, -1.000000000000000000, 0.000000000000000000 ) ) ;
#354 = DIRECTION ( 'NONE',  ( -0.9579671649362033747, 0.000000000000000000, 0.2868778675745011220 ) ) ;
#355 = DIRECTION ( 'NONE',  ( 0.2490110332224846623, 0.000000000000000000, -0.9685006480810793850 ) ) ;
#356 = CARTESIAN_POINT ( 'NONE',  ( 14.93741582401050394, -8.328813464873949357, -16.31187028222389657 ) ) ;
#357 = VECTOR ( 'NONE', #20266, 1000.000000000000000 ) ;
#358 = CARTESIAN_POINT ( 'NONE',  ( 12.25799425556778388, 34.52875999999999834, 0.2069032437451798767 ) ) ;
#359 = CARTESIAN_POINT ( 'NONE',  ( 10.92996571811956308, 19.50708099122125816, 6.637236655515030392 ) ) ;
#360 = EDGE_CURVE ( 'NONE', #21347, #13814, #17389, .T. ) ;
#361 = CARTESIAN_POINT ( 'NONE',  ( 14.73791976308111451, 13.08957250000000094, -17.32306410839158772 ) ) ;
#362 = EDGE_CURVE ( 'NONE', #10171, #5161, #12705, .T. ) ;
#363 = CARTESIAN_POINT ( 'NONE',  ( 11.51451690588786292, 12.10267245616517684, -1.401170015314361583 ) ) ;
#364 = LINE ( 'NONE', #8871, #4198 ) ;
#366 = CARTESIAN_POINT ( 'NONE',  ( -53.00154558624916490, -5.714999999999999858, -22.85927301266823264 ) ) ;
#365 = CARTESIAN_POINT ( 'NONE',  ( -0.3966899150635756488, 20.30256849354482185, 4.863884106276985086 ) ) ;
#367 = VERTEX_POINT ( 'NONE', #5509 ) ;
#368 = APPLICATION_PROTOCOL_DEFINITION ( 'draft international standard', 'automotive_design', 1998, #19056 ) ;
#369 = DIRECTION ( 'NONE',  ( -0.9964481331860212121, 0.000000000000000000, 0.08420877549337300871 ) ) ;
#370 = CARTESIAN_POINT ( 'NONE',  ( 4.663792239772604376, 20.04349882488605417, 1.216183641137849936 ) ) ;
#371 = DIRECTION ( 'NONE',  ( -0.7421532822901579785, 0.000000000000000000, 0.6702301885068630005 ) ) ;
#372 = AXIS2_PLACEMENT_3D ( 'NONE', #2270, #15784, #5467 ) ;
#373 = CARTESIAN_POINT ( 'NONE',  ( 41.45112526417833010, -1.983739999999999837, 7.778260066349530710 ) ) ;
#374 = VERTEX_POINT ( 'NONE', #3870 ) ;
#375 = CARTESIAN_POINT ( 'NONE',  ( 9.387588499473343617, 14.88153510792360024, 7.075887779341390349 ) ) ;
#376 = CARTESIAN_POINT ( 'NONE',  ( 4.517629800827023701, 19.79998728558659238, 6.347442110243458835 ) ) ;
#377 = VECTOR ( 'NONE', #1528, 1000.000000000000000 ) ;
#378 = CARTESIAN_POINT ( 'NONE',  ( 9.134405411020685150, 21.15227197021270200, 1.760129399948058282 ) ) ;
#379 = CARTESIAN_POINT ( 'NONE',  ( 1.869769858248796046, 17.31795573271877942, 9.441083779479226834 ) ) ;
#380 = CARTESIAN_POINT ( 'NONE',  ( 5.428607670497170190, 17.41093948017483939, -2.167354582218313563 ) ) ;
#381 = CIRCLE ( 'NONE', #12045, 4.365625000000000533 ) ;
#382 = VECTOR ( 'NONE', #11141, 1000.000000000000000 ) ;
#383 = CARTESIAN_POINT ( 'NONE',  ( 17.10576967688479399, -14.84248999999999974, -11.38708898545455561 ) ) ;
#384 = CARTESIAN_POINT ( 'NONE',  ( 11.42192246508016140, -4.515843507428392023, -15.23392906717917228 ) ) ;
#385 = ORIENTED_EDGE ( 'NONE', *, *, #5454, .T. ) ;
#386 = CARTESIAN_POINT ( 'NONE',  ( 11.18374392228187908, 14.11224683893468068, 6.306351795193365639 ) ) ;
#387 = CARTESIAN_POINT ( 'NONE',  ( 10.92933365986669259, 16.27139426067511607, -4.476694603249527837 ) ) ;
#388 = ORIENTED_EDGE ( 'NONE', *, *, #17748, .F. ) ;
#389 = EDGE_CURVE ( 'NONE', #18438, #18286, #10607, .T. ) ;
#390 = CARTESIAN_POINT ( 'NONE',  ( 10.37510084784339703, 11.39042657884375309, 2.489853968234712500 ) ) ;
#391 = LINE ( 'NONE', #12123, #16283 ) ;
#392 = DIRECTION ( 'NONE',  ( -0.7421532822901579785, 0.000000000000000000, 0.6702301885068628895 ) ) ;
#394 = FACE_OUTER_BOUND ( 'NONE', #19852, .T. ) ;
#393 = CARTESIAN_POINT ( 'NONE',  ( 3.768687125443949348, 21.23176840745776062, 5.325114473994855935 ) ) ;
#395 = VERTEX_POINT ( 'NONE', #5841 ) ;
#396 = CARTESIAN_POINT ( 'NONE',  ( 7.546623658496745435, 15.46605242080309850, 8.328871668325708910 ) ) ;
#397 = AXIS2_PLACEMENT_3D ( 'NONE', #13888, #8758, #15657 ) ;
#398 = DIRECTION ( 'NONE',  ( 0.4857267349359797870, 0.000000000000000000, -0.8741107132214044340 ) ) ;
#399 = AXIS2_PLACEMENT_3D ( 'NONE', #8708, #17541, #7472 ) ;
#400 = ORIENTED_EDGE ( 'NONE', *, *, #7902, .F. ) ;
#401 = VECTOR ( 'NONE', #4265, 1000.000000000000000 ) ;
#402 = CARTESIAN_POINT ( 'NONE',  ( 0.05840936790434386044, 16.18753194106394488, 0.7989642439863056111 ) ) ;
#403 = CARTESIAN_POINT ( 'NONE',  ( 29.45491884992628329, 34.52875999999999834, -15.58809351040512325 ) ) ;
#404 = ORIENTED_EDGE ( 'NONE', *, *, #18172, .T. ) ;
#405 = LINE ( 'NONE', #7160, #11390 ) ;
#406 = DIRECTION ( 'NONE',  ( -0.05085730733808142834, 0.000000000000000000, 0.9987059298363657467 ) ) ;
#407 = VECTOR ( 'NONE', #5440, 1000.000000000000000 ) ;
#408 = CARTESIAN_POINT ( 'NONE',  ( 1.923689137428217455, -0.9589899600121986056, -20.61772871637841220 ) ) ;
#409 = CARTESIAN_POINT ( 'NONE',  ( 64.66604708500285881, 32.54502000000000095, -11.54913207920052720 ) ) ;
#410 = VECTOR ( 'NONE', #17472, 1000.000000000000114 ) ;
#411 = VECTOR ( 'NONE', #16269, 1000.000000000000114 ) ;
#412 = ORIENTED_EDGE ( 'NONE', *, *, #11806, .F. ) ;
#413 = LINE ( 'NONE', #20514, #19877 ) ;
#414 = CARTESIAN_POINT ( 'NONE',  ( 17.22522857595987844, 34.52875999999999834, -15.04442098945225403 ) ) ;
#416 = CARTESIAN_POINT ( 'NONE',  ( 19.10984178700001479, -5.369063563745102741, -14.24189854854983217 ) ) ;
#415 = CARTESIAN_POINT ( 'NONE',  ( -6.268352501591477832, 33.32892749999999893, -35.49402737582407497 ) ) ;
#417 = ORIENTED_EDGE ( 'NONE', *, *, #10498, .T. ) ;
#418 = EDGE_LOOP ( 'NONE', ( #15231, #7592, #4547, #16029 ) ) ;
#419 = EDGE_CURVE ( 'NONE', #13188, #14728, #15986, .T. ) ;
#420 = VECTOR ( 'NONE', #6179, 1000.000000000000114 ) ;
#421 = CARTESIAN_POINT ( 'NONE',  ( 12.79548546626584127, 18.46234326053249220, 6.094044533436631994 ) ) ;
#422 = AXIS2_PLACEMENT_3D ( 'NONE', #16207, #16521, #8217 ) ;
#424 = LINE ( 'NONE', #13819, #15988 ) ;
#423 = CARTESIAN_POINT ( 'NONE',  ( 5.508019599735664684, 17.51021144529294560, 8.768403766408770394 ) ) ;
#425 = EDGE_LOOP ( 'NONE', ( #3626, #10707, #4614, #14152, #12802, #17035 ) ) ;
#426 = CARTESIAN_POINT ( 'NONE',  ( 4.517480175593667546, 11.08280834804601156, 3.521422171990641559 ) ) ;
#427 = ORIENTED_EDGE ( 'NONE', *, *, #17403, .F. ) ;
#428 = ORIENTED_EDGE ( 'NONE', *, *, #17879, .F. ) ;
#429 = CARTESIAN_POINT ( 'NONE',  ( 7.502072049523423658, 16.67234806097842892, -2.119060137569175772 ) ) ;
#430 = AXIS2_PLACEMENT_3D ( 'NONE', #13044, #6387, #21198 ) ;
#431 = VECTOR ( 'NONE', #2432, 1000.000000000000114 ) ;
#432 = EDGE_LOOP ( 'NONE', ( #13598, #21453 ) ) ;
#433 = CARTESIAN_POINT ( 'NONE',  ( 3.419769351041428873, 15.73143490412445900, 8.402936401063445970 ) ) ;
#434 = CIRCLE ( 'NONE', #1505, 0.5080000000000006732 ) ;
#435 = CARTESIAN_POINT ( 'NONE',  ( 28.87608719841374949, 1.975802500000001904, -15.73691681567849976 ) ) ;
#436 = VECTOR ( 'NONE', #9326, 1000.000000000000000 ) ;
#437 = EDGE_CURVE ( 'NONE', #16850, #6939, #17013, .T. ) ;
#438 = CARTESIAN_POINT ( 'NONE',  ( 31.83819605565793509, 34.52875999999999834, -4.158220719828246814 ) ) ;
#439 = DIRECTION ( 'NONE',  ( 0.8943161143440100380, 0.000000000000000000, 0.4474356798743612806 ) ) ;
#440 = LINE ( 'NONE', #5512, #18865 ) ;
#441 = CARTESIAN_POINT ( 'NONE',  ( 1.954711710866990693, 21.15578882893498047, 5.227293067434886531 ) ) ;
#442 = DIRECTION ( 'NONE',  ( -0.2868778675745010664, 0.000000000000000000, -0.9579671649362032637 ) ) ;
#443 = ORIENTED_EDGE ( 'NONE', *, *, #13997, .T. ) ;
#444 = CARTESIAN_POINT ( 'NONE',  ( 2.034109762226206541, 15.64505045901557345, 9.146289368853217638 ) ) ;
#445 = CARTESIAN_POINT ( 'NONE',  ( 17.87574706213523612, -3.968114999999999615, -11.18912023382283571 ) ) ;
#446 = DIRECTION ( 'NONE',  ( -0.2490110332224846346, 0.000000000000000000, 0.9685006480810792739 ) ) ;
#447 = CARTESIAN_POINT ( 'NONE',  ( -29.36874999999999858, 0.000000000000000000, -3.968750000000000000 ) ) ;
#448 = CARTESIAN_POINT ( 'NONE',  ( 55.81697695389291169, -14.84248999999999974, -11.14520323105768362 ) ) ;
#449 = AXIS2_PLACEMENT_3D ( 'NONE', #12581, #16021, #15571 ) ;
#450 = ORIENTED_EDGE ( 'NONE', *, *, #19358, .T. ) ;
#451 = ADVANCED_FACE ( 'NONE', ( #15819 ), #9149, .F. ) ;
#452 = CARTESIAN_POINT ( 'NONE',  ( 8.728086753073649007, 15.35048014666334559, -3.127714312744253711 ) ) ;
#453 = ADVANCED_FACE ( 'NONE', ( #15932 ), #20761, .T. ) ;
#454 = EDGE_CURVE ( 'NONE', #9720, #5388, #7845, .T. ) ;
#455 = DIRECTION ( 'NONE',  ( 0.000000000000000000, 1.000000000000000000, 0.000000000000000000 ) ) ;
#456 = CARTESIAN_POINT ( 'NONE',  ( 13.18577270084679576, 12.49465483329842286, 5.809243337312416600 ) ) ;
#457 = ORIENTED_EDGE ( 'NONE', *, *, #18854, .F. ) ;
#458 = ORIENTED_EDGE ( 'NONE', *, *, #17617, .T. ) ;
#459 = CIRCLE ( 'NONE', #9260, 0.5079999999999973426 ) ;
#460 = CARTESIAN_POINT ( 'NONE',  ( -15.84035234298960049, -2.442431200715369677, -10.46642885967791692 ) ) ;
#461 = CARTESIAN_POINT ( 'NONE',  ( 9.262764579346530525, 18.14018762746578517, 7.695032825047638525 ) ) ;
#462 = AXIS2_PLACEMENT_3D ( 'NONE', #21471, #19700, #9852 ) ;
#463 = CARTESIAN_POINT ( 'NONE',  ( 0.2422206219147293726, 20.17819236544972128, 6.176747626244641687 ) ) ;
#464 = CARTESIAN_POINT ( 'NONE',  ( 11.56192577415882816, -1.983739999999999393, 4.677561850332325299 ) ) ;
#465 = CARTESIAN_POINT ( 'NONE',  ( 5.857566774899138906, 18.14988412973438159, -1.063936251482671569 ) ) ;
#466 = DIRECTION ( 'NONE',  ( -0.4857267349359799535, 0.000000000000000000, 0.8741107132214044340 ) ) ;
#467 = CARTESIAN_POINT ( 'NONE',  ( 8.463232041149611362, 10.77439257666578243, 1.655928866917091069 ) ) ;
#468 = EDGE_CURVE ( 'NONE', #14260, #16212, #12495, .T. ) ;
#469 = CARTESIAN_POINT ( 'NONE',  ( 1.877249823927544359, 13.01816804744978207, 0.3577989692409621059 ) ) ;
#470 = CARTESIAN_POINT ( 'NONE',  ( 1.260594148623912059, 18.90536103616748775, 8.891112515372604719 ) ) ;
#471 = PRODUCT_DEFINITION ( 'UNKNOWN', '', #9128, #21835 ) ;
#472 = CARTESIAN_POINT ( 'NONE',  ( 19.75964483560148466, 0.004337915005267487314, -14.87722094040863752 ) ) ;
#473 = CARTESIAN_POINT ( 'NONE',  ( 7.221254323107455519, 13.47081914689558069, 6.792995896567122216 ) ) ;
#474 = DIRECTION ( 'NONE',  ( 0.2490110332224850231, 0.000000000000000000, -0.9685006480810791629 ) ) ;
#475 = CARTESIAN_POINT ( 'NONE',  ( 29.64606458365116737, -7.547927499999999235, -15.53894806404596096 ) ) ;
#476 = CARTESIAN_POINT ( 'NONE',  ( 17.01227936190448986, 2.147986159030752962, -15.15785924608550950 ) ) ;
#477 = PLANE ( 'NONE',  #19448 ) ;
#478 = EDGE_CURVE ( 'NONE', #18112, #12175, #19125, .T. ) ;
#479 = CARTESIAN_POINT ( 'NONE',  ( 10.83806774996162403, 19.83502426011275688, 6.410176537624181492 ) ) ;
#480 = ORIENTED_EDGE ( 'NONE', *, *, #17479, .T. ) ;
#481 = VECTOR ( 'NONE', #15576, 1000.000000000000000 ) ;
#482 = CARTESIAN_POINT ( 'NONE',  ( 30.97944403357121956, -1.983739999999999837, -8.103300075789407586 ) ) ;
#483 = CARTESIAN_POINT ( 'NONE',  ( 11.29923878586181196, 13.07119654552437638, -2.429333208372020270 ) ) ;
#484 = CARTESIAN_POINT ( 'NONE',  ( 14.83746136476627520, -7.423169472682626058, -15.14267033774566684 ) ) ;
#485 = ORIENTED_EDGE ( 'NONE', *, *, #3071, .F. ) ;
#486 = ITEM_DEFINED_TRANSFORMATION ( 'NONE', 'NONE', #6297,  #2234 ) ;
#487 = DIRECTION ( 'NONE',  ( -0.2490110332224846346, 0.000000000000000000, 0.9685006480810792739 ) ) ;
#488 = AXIS2_PLACEMENT_3D ( 'NONE', #287, #69, #10464 ) ;
#489 = DIRECTION ( 'NONE',  ( -0.9685006480810794960, 0.000000000000000000, -0.2490110332224836354 ) ) ;
#490 = VERTEX_POINT ( 'NONE', #7825 ) ;
#491 = CARTESIAN_POINT ( 'NONE',  ( 9.758652622545607613, 18.90452467200534414, -2.337483130687342925 ) ) ;
#492 = EDGE_CURVE ( 'NONE', #3590, #2498, #6272, .T. ) ;
#493 = CIRCLE ( 'NONE', #844, 1.190625000000000711 ) ;
#494 = CARTESIAN_POINT ( 'NONE',  ( 12.27885220188135484, 20.89247853322200044, -1.186209537071461151 ) ) ;
#495 = CARTESIAN_POINT ( 'NONE',  ( 1.550445315360883258, 21.03017768341116067, 3.245805655982831439 ) ) ;
#496 = EDGE_CURVE ( 'NONE', #17843, #3371, #1299, .T. ) ;
#497 = CARTESIAN_POINT ( 'NONE',  ( 11.09799212544334246, 12.31865010030356089, -2.962437906143603250 ) ) ;
#498 = EDGE_CURVE ( 'NONE', #10812, #21347, #20182, .T. ) ;
#499 = CARTESIAN_POINT ( 'NONE',  ( 53.14266576735298031, -7.546379553159687781, -16.66242751532464084 ) ) ;
#500 = CARTESIAN_POINT ( 'NONE',  ( 13.67756757867809725, 38.48766750000000059, 2.571257636385987144 ) ) ;
#501 = EDGE_LOOP ( 'NONE', ( #16352, #7920, #20206, #7975 ) ) ;
#502 = CARTESIAN_POINT ( 'NONE',  ( 6.897255242458841806, 21.59165172380602371, 1.391285824881070221 ) ) ;
#503 = VECTOR ( 'NONE', #5511, 1000.000000000000227 ) ;
#504 = CARTESIAN_POINT ( 'NONE',  ( 52.39214030333819494, 39.62760010306434566, -17.41425762687993029 ) ) ;
#505 = ORIENTED_EDGE ( 'NONE', *, *, #10172, .T. ) ;
#506 = CARTESIAN_POINT ( 'NONE',  ( 10.05115496733982638, 11.45101544124467097, 1.083611332447474540 ) ) ;
#507 = DIRECTION ( 'NONE',  ( 0.000000000000000000, -1.000000000000000000, 0.000000000000000000 ) ) ;
#508 = CARTESIAN_POINT ( 'NONE',  ( 19.07578797920377411, 34.51447250000000366, -18.25667004382573566 ) ) ;
#510 = FACE_OUTER_BOUND ( 'NONE', #6893, .T. ) ;
#509 = CARTESIAN_POINT ( 'NONE',  ( 2.579550200575633223, 11.32322398379630179, 5.299602097076567375 ) ) ;
#511 = ORIENTED_EDGE ( 'NONE', *, *, #13513, .F. ) ;
#512 = DIRECTION ( 'NONE',  ( 0.1060008583745224581, 0.000000000000000000, 0.9943660382494288186 ) ) ;
#513 = VERTEX_POINT ( 'NONE', #11150 ) ;
#514 = DIRECTION ( 'NONE',  ( -0.9685006480810792739, 0.000000000000000000, -0.2490110332224850509 ) ) ;
#515 = CARTESIAN_POINT ( 'NONE',  ( 19.96989445820344855, -1.596441888161631573, -15.57706592207198781 ) ) ;
#516 = ORIENTED_EDGE ( 'NONE', *, *, #17729, .F. ) ;
#517 = CARTESIAN_POINT ( 'NONE',  ( 1.670997140563193373, 34.12394749999999988, -22.76294857149378714 ) ) ;
#518 = AXIS2_PLACEMENT_3D ( 'NONE', #7879, #21361, #11096 ) ;
#519 = ADVANCED_FACE ( 'NONE', ( #14481 ), #16142, .F. ) ;
#520 = CARTESIAN_POINT ( 'NONE',  ( 46.03750000000000142, -14.84248999999999974, -10.31874999999999964 ) ) ;
#521 = AXIS2_PLACEMENT_3D ( 'NONE', #15161, #6738, #13502 ) ;
#522 = CARTESIAN_POINT ( 'NONE',  ( 14.43917063414567536, 39.28268749999999443, 2.343183994106907697 ) ) ;
#523 = DIRECTION ( 'NONE',  ( 0.7421532822901579785, 0.000000000000000000, -0.6702301885068630005 ) ) ;
#524 = EDGE_LOOP ( 'NONE', ( #10286, #14452, #3255, #19034 ) ) ;
#525 = CARTESIAN_POINT ( 'NONE',  ( 59.65121809612895731, 0.000000000000000000, -2.485718937265306572 ) ) ;
#526 = CARTESIAN_POINT ( 'NONE',  ( 1.998220421679061776, 25.39269750000000059, -22.64748046904500356 ) ) ;
#527 = CARTESIAN_POINT ( 'NONE',  ( 59.86950051480232560, -6.356984999999999886, -17.89453710146031185 ) ) ;
#529 = CARTESIAN_POINT ( 'NONE',  ( 14.96245394991857580, -7.172648401804374352, -15.07977408558167731 ) ) ;
#528 = CARTESIAN_POINT ( 'NONE',  ( 46.03750000000000142, 0.000000000000000000, -10.31874999999999964 ) ) ;
#530 = ORIENTED_EDGE ( 'NONE', *, *, #8325, .F. ) ;
#531 = ORIENTED_EDGE ( 'NONE', *, *, #4323, .T. ) ;
#532 = CARTESIAN_POINT ( 'NONE',  ( 12.33551329399142915, 11.22339177084746176, 2.585388245275515917 ) ) ;
#534 = DIRECTION ( 'NONE',  ( 0.7334850928793772429, -0.6768732144311024879, -0.06198604769977036216 ) ) ;
#533 = CARTESIAN_POINT ( 'NONE',  ( 2.840321306701502291, 20.92456416987101875, 1.832874750768024086 ) ) ;
#535 = VERTEX_POINT ( 'NONE', #17898 ) ;
#537 = CARTESIAN_POINT ( 'NONE',  ( 11.61240041076558960, -6.892588391211154963, -15.33507383697825688 ) ) ;
#536 = CARTESIAN_POINT ( 'NONE',  ( 4.164513427734910067, 11.38116224488952177, 2.006366593415208399 ) ) ;
#538 = ORIENTED_EDGE ( 'NONE', *, *, #3166, .T. ) ;
#539 = VERTEX_POINT ( 'NONE', #21310 ) ;
#540 = CARTESIAN_POINT ( 'NONE',  ( 7.555449444248006685, 13.41026002100023184, -1.138537544275743274 ) ) ;
#541 = AXIS2_PLACEMENT_3D ( 'NONE', #1411, #17800, #2648 ) ;
#542 = ORIENTED_EDGE ( 'NONE', *, *, #52, .F. ) ;
#543 = CARTESIAN_POINT ( 'NONE',  ( 3.211736503681509980, 12.96355677795110140, 6.856356644963555347 ) ) ;
#544 = EDGE_CURVE ( 'NONE', #7495, #1968, #3265, .T. ) ;
#545 = CARTESIAN_POINT ( 'NONE',  ( 46.03750000000000142, -3.968114999999999615, -10.31874999999999964 ) ) ;
#546 = CARTESIAN_POINT ( 'NONE',  ( 38.94885947252247860, -7.547248457916676756, -3.956611957470116625 ) ) ;
#547 = DIRECTION ( 'NONE',  ( 0.000000000000000000, 1.000000000000000000, 0.000000000000000000 ) ) ;
#548 = CARTESIAN_POINT ( 'NONE',  ( 1.864588651777728590, 21.18383126686373430, 4.984355216872713434 ) ) ;
#549 = ORIENTED_EDGE ( 'NONE', *, *, #989, .F. ) ;
#550 = CARTESIAN_POINT ( 'NONE',  ( 5.577949907072537350, 17.33943586079730181, 8.015011952332226741 ) ) ;
#551 = DIRECTION ( 'NONE',  ( 0.000000000000000000, -1.000000000000000000, 0.000000000000000000 ) ) ;
#552 = LINE ( 'NONE', #7622, #13154 ) ;
#553 = DIRECTION ( 'NONE',  ( -0.8583349619704310207, 0.000000000000000000, 0.5130897514657826175 ) ) ;
#554 = CIRCLE ( 'NONE', #4091, 0.3962399999999999811 ) ;
#555 = DIRECTION ( 'NONE',  ( 0.000000000000000000, 1.000000000000000000, 0.000000000000000000 ) ) ;
#556 = ADVANCED_FACE ( 'NONE', ( #9374 ), #2746, .T. ) ;
#557 = ORIENTED_EDGE ( 'NONE', *, *, #19024, .T. ) ;
#558 = ORIENTED_EDGE ( 'NONE', *, *, #17949, .F. ) ;
#559 = CARTESIAN_POINT ( 'NONE',  ( 8.185500201082774652, 11.14036371107460255, 3.740216416401582755 ) ) ;
#560 = SHAPE_REPRESENTATION ( 'Handle Latch Pawl Plate', ( #2234 ), #14439 ) ;
#561 = CARTESIAN_POINT ( 'NONE',  ( 22.02657784715807665, 128.5105379999999968, -12.98906981665815330 ) ) ;
#562 = CARTESIAN_POINT ( 'NONE',  ( 11.75539605838384638, 10.66431821468159136, -0.2581068381348511354 ) ) ;
#563 = ORIENTED_EDGE ( 'NONE', *, *, #17228, .T. ) ;
#564 = EDGE_LOOP ( 'NONE', ( #7716, #9815, #9669, #1208 ) ) ;
#565 = PLANE ( 'NONE',  #6360 ) ;
#566 = CARTESIAN_POINT ( 'NONE',  ( 7.725504655093541118, 11.48266921152324116, -0.1321688645820411623 ) ) ;
#567 = CARTESIAN_POINT ( 'NONE',  ( 4.559726464520669431, 19.87799086262558035, 6.390853160755138873 ) ) ;
#568 = CARTESIAN_POINT ( 'NONE',  ( 64.14292646034530776, -1.983739999999999837, -12.24881465648521939 ) ) ;
#569 = CARTESIAN_POINT ( 'NONE',  ( 5.638166626312271390, 14.02190832120166775, -0.7723171704840984253 ) ) ;
#570 = EDGE_CURVE ( 'NONE', #16730, #6476, #8894, .T. ) ;
#571 = CARTESIAN_POINT ( 'NONE',  ( 0.9615939815707198468, 19.83869222877949667, 2.643595094647703370 ) ) ;
#572 = PLANE ( 'NONE',  #16036 ) ;
#573 = EDGE_CURVE ( 'NONE', #9259, #10436, #9589, .T. ) ;
#574 = CARTESIAN_POINT ( 'NONE',  ( 14.39495272017181016, 21.28532635717934340, 3.392014037587451458 ) ) ;
#575 = ADVANCED_FACE ( 'NONE', ( #16250 ), #19549, .F. ) ;
#576 = CARTESIAN_POINT ( 'NONE',  ( 4.913515329053552705, 12.19104956382561689, 5.302203639509063038 ) ) ;
#577 = CARTESIAN_POINT ( 'NONE',  ( 3.777435572934427110, 12.19982130767714246, 0.3897271289892410562 ) ) ;
#578 = CARTESIAN_POINT ( 'NONE',  ( -5.536601939709260733, 3.961447500000001565, -30.39452380949970944 ) ) ;
#579 = DIRECTION ( 'NONE',  ( -0.9964481331860213231, 0.000000000000000000, 0.08420877549337293932 ) ) ;
#580 = CARTESIAN_POINT ( 'NONE',  ( 4.502328515861612424, 19.89758433537658178, 0.8700102451280966598 ) ) ;
#581 = CARTESIAN_POINT ( 'NONE',  ( 29.19635173153840313, 32.54502000000000095, -6.218966092919240296 ) ) ;
#582 = FACE_BOUND ( 'NONE', #7037, .T. ) ;
#583 = CARTESIAN_POINT ( 'NONE',  ( 19.69663990328241354, 0.4662939914211877701, -14.34639758507740304 ) ) ;
#584 = CARTESIAN_POINT ( 'NONE',  ( 52.91086381164393515, 2.586003464000000029, 3.812938856729753301 ) ) ;
#585 = CARTESIAN_POINT ( 'NONE',  ( 9.969205024995844155, 10.71176808653972223, 0.7780162768078369151 ) ) ;
#586 = ORIENTED_EDGE ( 'NONE', *, *, #10826, .T. ) ;
#587 = CARTESIAN_POINT ( 'NONE',  ( 49.41235866845560309, 32.54502000000000095, -26.78690084448080100 ) ) ;
#588 = CARTESIAN_POINT ( 'NONE',  ( 11.20238673225087211, 13.86092089083514800, -2.958941917828961543 ) ) ;
#589 = LINE ( 'NONE', #20695, #6002 ) ;
#590 = ORIENTED_EDGE ( 'NONE', *, *, #21010, .F. ) ;
#591 = APPLICATION_PROTOCOL_DEFINITION ( 'draft international standard', 'automotive_design', 1998, #8467 ) ;
#592 = EDGE_CURVE ( 'NONE', #19225, #19536, #1138, .T. ) ;
#593 = AXIS2_PLACEMENT_3D ( 'NONE', #12095, #15316, #1903 ) ;
#594 = CARTESIAN_POINT ( 'NONE',  ( -6.268352501600194415, -1.265494433635971250, -35.49402737582123990 ) ) ;
#595 = ORIENTED_EDGE ( 'NONE', *, *, #11225, .F. ) ;
#596 = CARTESIAN_POINT ( 'NONE',  ( 9.466445536643458780, 17.21895884409014599, -2.918710521388331092 ) ) ;
#597 = EDGE_CURVE ( 'NONE', #14787, #535, #13511, .T. ) ;
#598 = CARTESIAN_POINT ( 'NONE',  ( 4.551873131176118470, 19.73415439451352427, 6.433038573175717367 ) ) ;
#599 = CARTESIAN_POINT ( 'NONE',  ( 8.554937540587033595, 20.63193666139594029, 0.1873199234380305001 ) ) ;
#600 = CARTESIAN_POINT ( 'NONE',  ( 3.820173452861999053, 13.16763011922862070, 8.063327502814468417 ) ) ;
#601 = FACE_OUTER_BOUND ( 'NONE', #956, .T. ) ;
#602 = DIRECTION ( 'NONE',  ( 0.9129422336036122632, 0.000000000000000000, -0.4080888115384288528 ) ) ;
#603 = CARTESIAN_POINT ( 'NONE',  ( 14.47570345013334148, 0.8437009842499967327, -15.92338500342878937 ) ) ;
#604 = CARTESIAN_POINT ( 'NONE',  ( 13.37471192292826139, 17.58265891940030556, -17.38954468002155451 ) ) ;
#605 = ORIENTED_EDGE ( 'NONE', *, *, #6499, .F. ) ;
#606 = CARTESIAN_POINT ( 'NONE',  ( 11.21453129928410597, 15.64639171652562588, 6.772637486115957728 ) ) ;
#607 = CARTESIAN_POINT ( 'NONE',  ( 9.432974783129361995, 11.74680749646248223, -1.582753286535103499 ) ) ;
#608 = DIRECTION ( 'NONE',  ( 0.08420877549337300871, 0.000000000000000000, 0.9964481331860212121 ) ) ;
#609 = ORIENTED_EDGE ( 'NONE', *, *, #4647, .F. ) ;
#610 = CARTESIAN_POINT ( 'NONE',  ( 9.349647467888569707, 16.65363258022448179, -2.856910848570457961 ) ) ;
#611 = CARTESIAN_POINT ( 'NONE',  ( 30.25543876212147509, 34.52875999999999834, -19.39939755251907272 ) ) ;
#612 = CARTESIAN_POINT ( 'NONE',  ( 3.805353748838121053, -1.983739999999999393, -22.18284873352824960 ) ) ;
#614 = FACE_OUTER_BOUND ( 'NONE', #18678, .T. ) ;
#613 = CARTESIAN_POINT ( 'NONE',  ( 7.115219445481534066, 13.03499949018002191, 7.425824234857630657 ) ) ;
#615 = ORIENTED_EDGE ( 'NONE', *, *, #14572, .T. ) ;
#616 = CARTESIAN_POINT ( 'NONE',  ( 6.832388641462657120, 11.15782348525851120, 4.714514794290550981 ) ) ;
#617 = ADVANCED_FACE ( 'NONE', ( #11371 ), #19429, .T. ) ;
#618 = ADVANCED_FACE ( 'NONE', ( #9701 ), #12829, .F. ) ;
#619 = CYLINDRICAL_SURFACE ( 'NONE', #19701, 30.16249999999999076 ) ;
#620 = EDGE_CURVE ( 'NONE', #8192, #8377, #16467, .T. ) ;
#621 = EDGE_LOOP ( 'NONE', ( #5754, #17722, #15374, #17996, #9493, #4829, #6803, #12935, #19285, #5126, #563, #5731, #12820, #9699, #14120, #19790, #20475, #19543, #9154, #13893, #19426, #8672, #3701, #4027, #204, #17065, #19652, #9741, #16692, #2515, #19472, #8946, #13944, #4403, #14015, #10589, #1724, #609, #18551, #13398 ) ) ;
#622 = CARTESIAN_POINT ( 'NONE',  ( 65.90927232300019512, 0.000000000000000000, -13.30734117861468135 ) ) ;
#623 = CARTESIAN_POINT ( 'NONE',  ( 19.10610158472843167, -0.2473655220616398365, -14.45733488498617625 ) ) ;
#624 = VERTEX_POINT ( 'NONE', #4304 ) ;
#625 = CARTESIAN_POINT ( 'NONE',  ( 59.80894853325292360, -6.356984999999999886, -16.70545285374888778 ) ) ;
#626 = CARTESIAN_POINT ( 'NONE',  ( 17.99520596118501814, -14.84248999999999974, -14.84645223781840073 ) ) ;
#627 = FACE_OUTER_BOUND ( 'NONE', #9472, .T. ) ;
#628 = ORIENTED_EDGE ( 'NONE', *, *, #11808, .F. ) ;
#629 = CYLINDRICAL_SURFACE ( 'NONE', #3313, 0.3962399999999990929 ) ;
#630 = CARTESIAN_POINT ( 'NONE',  ( 1.952969610814715207, 8.739187247087119914, 8.731249999999999289 ) ) ;
#631 = ORIENTED_EDGE ( 'NONE', *, *, #14864, .T. ) ;
#632 = ORIENTED_EDGE ( 'NONE', *, *, #7507, .T. ) ;
#633 = AXIS2_PLACEMENT_3D ( 'NONE', #13523, #13632, #8307 ) ;
#635 = CARTESIAN_POINT ( 'NONE',  ( 7.735533989518945219, 5.548947500000001476, -21.17236077523805449 ) ) ;
#634 = CARTESIAN_POINT ( 'NONE',  ( 0.2965678313766248464, 20.95713891276306029, 6.390564738160584568 ) ) ;
#636 = ORIENTED_EDGE ( 'NONE', *, *, #7107, .T. ) ;
#638 = CARTESIAN_POINT ( 'NONE',  ( 11.79048631737284936, -6.033539481721004627, -16.29381363364702295 ) ) ;
#637 = CARTESIAN_POINT ( 'NONE',  ( 5.548917213503941070, 13.89478552866151695, 8.213063205195311411 ) ) ;
#639 = EDGE_CURVE ( 'NONE', #5833, #5959, #21527, .T. ) ;
#640 = ORIENTED_EDGE ( 'NONE', *, *, #20179, .T. ) ;
#641 = EDGE_CURVE ( 'NONE', #1856, #20988, #8151, .T. ) ;
#642 = ORIENTED_EDGE ( 'NONE', *, *, #17287, .T. ) ;
#643 = CARTESIAN_POINT ( 'NONE',  ( 1.460844719705742367, 14.43398395740774554, 8.397187112944255460 ) ) ;
#644 = ORIENTED_EDGE ( 'NONE', *, *, #3564, .T. ) ;
#645 = VECTOR ( 'NONE', #6896, 1000.000000000000114 ) ;
#646 = CARTESIAN_POINT ( 'NONE',  ( 18.74375446079810104, 0.5063334429457699848, 10.05646519131946093 ) ) ;
#647 = CARTESIAN_POINT ( 'NONE',  ( 19.07578797920376701, -3.966527499999997097, -18.25667004382573921 ) ) ;
#648 = DIRECTION ( 'NONE',  ( 0.000000000000000000, -1.000000000000000000, 0.000000000000000000 ) ) ;
#649 = CARTESIAN_POINT ( 'NONE',  ( 11.42842559562532578, -3.968114999999999615, 1.673196738795719174 ) ) ;
#650 = CARTESIAN_POINT ( 'NONE',  ( 3.604055471673875743, 16.46645633495994687, 9.203776892202039761 ) ) ;
#651 = ORIENTED_EDGE ( 'NONE', *, *, #18149, .F. ) ;
#652 =( GEOMETRIC_REPRESENTATION_CONTEXT ( 3 ) GLOBAL_UNCERTAINTY_ASSIGNED_CONTEXT ( ( #15443 ) ) GLOBAL_UNIT_ASSIGNED_CONTEXT ( ( #4485, #7792, #7584 ) ) REPRESENTATION_CONTEXT ( 'NONE', 'WORKASPACE' ) );
#653 = CARTESIAN_POINT ( 'NONE',  ( 7.000609123144855062, 19.58301787754098200, 6.453108639060604723 ) ) ;
#654 = CARTESIAN_POINT ( 'NONE',  ( 11.56051848560380435, -4.566074003843849205, -16.36139799744035628 ) ) ;
#655 = DIRECTION ( 'NONE',  ( 0.000000000000000000, 1.000000000000000000, 0.000000000000000000 ) ) ;
#656 = DIRECTION ( 'NONE',  ( 0.000000000000000000, -1.000000000000000000, 0.000000000000000000 ) ) ;
#657 = ORIENTED_EDGE ( 'NONE', *, *, #6799, .T. ) ;
#658 = ORIENTED_EDGE ( 'NONE', *, *, #14396, .F. ) ;
#659 = CARTESIAN_POINT ( 'NONE',  ( 7.358775753619412718, 11.69576222774042229, 0.1904761656118920121 ) ) ;
#661 = DIRECTION ( 'NONE',  ( 0.07875956036501312318, 0.000000000000000000, -0.9968936410927243807 ) ) ;
#660 = DIRECTION ( 'NONE',  ( 0.2490110332224846346, 0.000000000000000000, -0.9685006480810792739 ) ) ;
#662 = CARTESIAN_POINT ( 'NONE',  ( 11.28216995687987279, 11.80526944224940777, -2.285198803090960240 ) ) ;
#663 = ORIENTED_EDGE ( 'NONE', *, *, #15860, .F. ) ;
#664 = EDGE_LOOP ( 'NONE', ( #18136, #17984, #7800, #6958 ) ) ;
#665 = EDGE_CURVE ( 'NONE', #14162, #4933, #12805, .T. ) ;
#666 = LINE ( 'NONE', #20779, #7420 ) ;
#667 = CIRCLE ( 'NONE', #3491, 1.984375000000000000 ) ;
#668 = CARTESIAN_POINT ( 'NONE',  ( 7.246288661058416736, 14.17700572773325618, -2.455816413159584766 ) ) ;
#669 = CARTESIAN_POINT ( 'NONE',  ( 3.783282799006013164, 14.05198016149147122, -0.1472696480691887966 ) ) ;
#670 = CARTESIAN_POINT ( 'NONE',  ( 1.776692311944953584, 34.12394749999999988, -22.71488278333200839 ) ) ;
#671 = CARTESIAN_POINT ( 'NONE',  ( 6.022052921700177919, 18.85282495273109760, -0.7063640773682651197 ) ) ;
#672 = CARTESIAN_POINT ( 'NONE',  ( 37.13209340688868565, -6.356984999999999886, -3.529402718062123689 ) ) ;
#673 = VECTOR ( 'NONE', #3578, 1000.000000000000000 ) ;
#674 = EDGE_CURVE ( 'NONE', #1, #6701, #6424, .T. ) ;
#675 = CARTESIAN_POINT ( 'NONE',  ( 7.067964712802636384, 11.13551934581288094, 4.361396337857177841 ) ) ;
#676 = CARTESIAN_POINT ( 'NONE',  ( 4.643852685068835306, 11.88709150950850280, 4.078001338485435667 ) ) ;
#677 = CYLINDRICAL_SURFACE ( 'NONE', #11422, 0.3962400000000008138 ) ;
#678 = CARTESIAN_POINT ( 'NONE',  ( 2.864312977351492595, 11.23735775897588240, 5.231261027419050968 ) ) ;
#679 = DIRECTION ( 'NONE',  ( 0.2868778675745011220, 0.000000000000000000, 0.9579671649362033747 ) ) ;
#680 = AXIS2_PLACEMENT_3D ( 'NONE', #2628, #20743, #5925 ) ;
#681 = CARTESIAN_POINT ( 'NONE',  ( 14.14084833952063747, 15.36419388438619649, -16.93566361603518899 ) ) ;
#682 = CARTESIAN_POINT ( 'NONE',  ( 6.162093721932920154, 20.44527992609954126, 5.228833816242916654 ) ) ;
#683 = DIRECTION ( 'NONE',  ( 0.000000000000000000, 1.000000000000000000, 0.000000000000000000 ) ) ;
#684 = CARTESIAN_POINT ( 'NONE',  ( 38.23013820809905638, -9.531985000000000596, -14.22485453658974031 ) ) ;
#685 = CARTESIAN_POINT ( 'NONE',  ( 12.15102624612472404, 0.6667575905376122991, -16.60929033701790303 ) ) ;
#686 = FACE_OUTER_BOUND ( 'NONE', #17221, .T. ) ;
#687 = AXIS2_PLACEMENT_3D ( 'NONE', #15125, #6696, #20168 ) ;
#688 = CARTESIAN_POINT ( 'NONE',  ( 9.637199341109212725, 11.24896747874181280, -0.6285487678327054129 ) ) ;
#689 = ORIENTED_EDGE ( 'NONE', *, *, #13845, .F. ) ;
#690 = DIRECTION ( 'NONE',  ( -0.000000000000000000, -1.000000000000000000, 0.000000000000000000 ) ) ;
#691 = EDGE_CURVE ( 'NONE', #3431, #18275, #1843, .T. ) ;
#692 = CARTESIAN_POINT ( 'NONE',  ( 11.17252035512641406, 14.29393921748002505, -3.161770295153791821 ) ) ;
#693 = CARTESIAN_POINT ( 'NONE',  ( 5.366064009540067126, 15.47516136557390176, -2.081252157664847502 ) ) ;
#694 = CARTESIAN_POINT ( 'NONE',  ( -16.14706788831979978, 36.51313500000000545, -25.97380585690919830 ) ) ;
#695 = ORIENTED_EDGE ( 'NONE', *, *, #7242, .F. ) ;
#696 = CONTEXT_DEPENDENT_SHAPE_REPRESENTATION ( #16409, #7244 ) ;
#697 = LINE ( 'NONE', #19041, #16642 ) ;
#698 = CARTESIAN_POINT ( 'NONE',  ( 28.56548256563643662, -14.84248999999999974, -12.12873025803960658 ) ) ;
#699 = VERTEX_POINT ( 'NONE', #3620 ) ;
#700 = CARTESIAN_POINT ( 'NONE',  ( 13.16576134418140676, 13.22236995718078134, 5.489006338729662815 ) ) ;
#701 = AXIS2_PLACEMENT_3D ( 'NONE', #14633, #10960, #2564 ) ;
#702 = CARTESIAN_POINT ( 'NONE',  ( 7.448594639129619388, 14.64975276093931100, -1.928932895048531826 ) ) ;
#703 = DIRECTION ( 'NONE',  ( -0.4128958666089267981, 0.5884034904305870395, 0.6951966166390379787 ) ) ;
#704 = DIRECTION ( 'NONE',  ( 0.9784543669157820256, 0.000000000000000000, 0.2064631973583577473 ) ) ;
#705 = EDGE_CURVE ( 'NONE', #1101, #3875, #6823, .T. ) ;
#706 = CARTESIAN_POINT ( 'NONE',  ( 4.078297738883024159, 21.19975011080603977, 5.266598747592275309 ) ) ;
#707 = CARTESIAN_POINT ( 'NONE',  ( 14.70048594802655550, 0.9231428247525146347, -15.85394111059815891 ) ) ;
#708 = LINE ( 'NONE', #15884, #14164 ) ;
#709 = VECTOR ( 'NONE', #2797, 1000.000000000000000 ) ;
#710 = EDGE_LOOP ( 'NONE', ( #9718, #14667, #1796, #5850, #15920 ) ) ;
#711 = CARTESIAN_POINT ( 'NONE',  ( 11.21068335584656950, 15.75969117811444953, 6.785562080493880543 ) ) ;
#712 = CARTESIAN_POINT ( 'NONE',  ( 8.439759197263338564, 21.35170238401046205, -0.1649572212692822781 ) ) ;
#713 = FACE_OUTER_BOUND ( 'NONE', #15999, .T. ) ;
#714 = ORIENTED_EDGE ( 'NONE', *, *, #19357, .F. ) ;
#715 = ADVANCED_FACE ( 'NONE', ( #13584 ), #1729, .F. ) ;
#716 = CARTESIAN_POINT ( 'NONE',  ( 9.461280943800495891, 13.02742443158000185, -1.607818659218023027 ) ) ;
#717 = LINE ( 'NONE', #12670, #3287 ) ;
#718 = ADVANCED_FACE ( 'NONE', ( #1946 ), #18430, .T. ) ;
#719 = ADVANCED_FACE ( 'NONE', ( #3305 ), #10243, .F. ) ;
#720 = CIRCLE ( 'NONE', #9536, 0.7950200000000005041 ) ;
#722 = LINE ( 'NONE', #20832, #16647 ) ;
#721 = CARTESIAN_POINT ( 'NONE',  ( 5.979923096379600622, 10.94213887786034078, 2.451138684234262843 ) ) ;
#723 = VERTEX_POINT ( 'NONE', #3504 ) ;
#724 = CARTESIAN_POINT ( 'NONE',  ( 7.260258248780015577, 12.25695181527388478, 6.604289441735033073 ) ) ;
#725 = CYLINDRICAL_SURFACE ( 'NONE', #8862, 20.83593749999999289 ) ;
#726 = CARTESIAN_POINT ( 'NONE',  ( 1.268730000000000135, 9.129395000000000593, 8.609509071587499562 ) ) ;
#727 = ORIENTED_EDGE ( 'NONE', *, *, #2466, .F. ) ;
#728 = DIRECTION ( 'NONE',  ( 0.000000000000000000, 1.000000000000000000, 0.000000000000000000 ) ) ;
#729 = CIRCLE ( 'NONE', #7799, 2.381250000000001421 ) ;
#730 = CARTESIAN_POINT ( 'NONE',  ( 11.61321856100838446, -3.658181173652626850, -15.64410391039172765 ) ) ;
#731 = EDGE_LOOP ( 'NONE', ( #7711, #2068 ) ) ;
#732 = LINE ( 'NONE', #7593, #11396 ) ;
#733 = AXIS2_PLACEMENT_3D ( 'NONE', #2522, #9471, #14263 ) ;
#734 = DIRECTION ( 'NONE',  ( 0.3928209820863007851, 0.000000000000000000, -0.9196149607486571176 ) ) ;
#735 = EDGE_CURVE ( 'NONE', #12688, #16536, #11693, .T. ) ;
#736 = VERTEX_POINT ( 'NONE', #11907 ) ;
#737 = CARTESIAN_POINT ( 'NONE',  ( -46.55773479047372376, 43.41875999999999891, -7.870535429687039120 ) ) ;
#738 = LINE ( 'NONE', #19310, #21439 ) ;
#739 = VECTOR ( 'NONE', #11879, 1000.000000000000000 ) ;
#740 = ORIENTED_EDGE ( 'NONE', *, *, #20509, .F. ) ;
#741 = ORIENTED_EDGE ( 'NONE', *, *, #1772, .T. ) ;
#742 = VECTOR ( 'NONE', #16555, 1000.000000000000114 ) ;
#743 = ADVANCED_FACE ( 'NONE', ( #9913 ), #18750, .T. ) ;
#745 = LINE ( 'NONE', #16241, #21205 ) ;
#744 = CARTESIAN_POINT ( 'NONE',  ( 4.406439411525544081, 20.54241105020114233, 0.3878223501788354843 ) ) ;
#746 = CIRCLE ( 'NONE', #9211, 0.5079999999999996740 ) ;
#747 = EDGE_LOOP ( 'NONE', ( #450, #19069, #6393, #18964 ) ) ;
#748 = CARTESIAN_POINT ( 'NONE',  ( 5.161554602150648208, 11.81472031015017166, 6.306168054739473838 ) ) ;
#749 = ORIENTED_EDGE ( 'NONE', *, *, #21150, .T. ) ;
#750 = EDGE_LOOP ( 'NONE', ( #6315, #10700, #9277, #2077, #19066, #6524 ) ) ;
#751 = PRESENTATION_LAYER_ASSIGNMENT (  '', '', ( #11690 ) ) ;
#752 = CARTESIAN_POINT ( 'NONE',  ( 1.284022825976741000, 13.11577469953204655, 7.340846339184095903 ) ) ;
#753 = ORIENTED_EDGE ( 'NONE', *, *, #1834, .F. ) ;
#754 = AXIS2_PLACEMENT_3D ( 'NONE', #7235, #13993, #4124 ) ;
#755 = AXIS2_PLACEMENT_3D ( 'NONE', #8975, #21028, #5874 ) ;
#756 = CIRCLE ( 'NONE', #19475, 0.5079999999999985638 ) ;
#757 = CARTESIAN_POINT ( 'NONE',  ( 6.472296726610020201, 0.08030987734106199982, 9.295161179239141092 ) ) ;
#758 = EDGE_CURVE ( 'NONE', #20373, #1329, #18433, .T. ) ;
#759 = CYLINDRICAL_SURFACE ( 'NONE', #18143, 3.970019999999997662 ) ;
#760 = DIRECTION ( 'NONE',  ( 0.000000000000000000, -1.000000000000000000, 0.000000000000000000 ) ) ;
#761 = CARTESIAN_POINT ( 'NONE',  ( 1.635490509552675942, 21.19865827025175520, 4.366209288297318025 ) ) ;
#762 = ADVANCED_FACE ( 'NONE', ( #16785 ), #13268, .T. ) ;
#763 = AXIS2_PLACEMENT_3D ( 'NONE', #1873, #5290, #4872 ) ;
#764 = EDGE_CURVE ( 'NONE', #7013, #13795, #15358, .T. ) ;
#765 = ORIENTED_EDGE ( 'NONE', *, *, #8954, .T. ) ;
#766 = CARTESIAN_POINT ( 'NONE',  ( 1.821934098042296446, 12.85015660565266060, 7.648703090803636861 ) ) ;
#767 = CARTESIAN_POINT ( 'NONE',  ( 10.76290084369569300, -4.809670885807078911, -16.11272035331650088 ) ) ;
#768 = DIRECTION ( 'NONE',  ( 0.2868778675745004558, 0.000000000000000000, 0.9579671649362035968 ) ) ;
#769 = CARTESIAN_POINT ( 'NONE',  ( 20.91979369334982053, -1.192140601152523738, -15.67394038340841433 ) ) ;
#770 = CARTESIAN_POINT ( 'NONE',  ( 55.33978576324753362, 0.000000000000000000, -23.05096232720518756 ) ) ;
#771 = EDGE_LOOP ( 'NONE', ( #6023, #8487, #4066, #14596 ) ) ;
#772 = ORIENTED_EDGE ( 'NONE', *, *, #5768, .T. ) ;
#773 = CARTESIAN_POINT ( 'NONE',  ( 12.82931649728759282, 16.73453105516203721, 7.016643571353146314 ) ) ;
#775 = LINE ( 'NONE', #19445, #8515 ) ;
#774 = DIRECTION ( 'NONE',  ( 0.000000000000000000, 1.000000000000000000, 0.000000000000000000 ) ) ;
#776 = CARTESIAN_POINT ( 'NONE',  ( 12.88484886689720810, 11.29734215691586208, 4.459301396266069695 ) ) ;
#777 = VERTEX_POINT ( 'NONE', #19975 ) ;
#778 = AXIS2_PLACEMENT_3D ( 'NONE', #1408, #18118, #2976 ) ;
#779 = ORIENTED_EDGE ( 'NONE', *, *, #14955, .F. ) ;
#780 = DIRECTION ( 'NONE',  ( 0.000000000000000000, 1.000000000000000000, 0.000000000000000000 ) ) ;
#781 = AXIS2_PLACEMENT_3D ( 'NONE', #4089, #977, #12506 ) ;
#782 = AXIS2_PLACEMENT_3D ( 'NONE', #19094, #1965, #3522 ) ;
#783 = CARTESIAN_POINT ( 'NONE',  ( 7.240898627860822501, 16.21294576777124519, -2.887031719764514115 ) ) ;
#784 = DIRECTION ( 'NONE',  ( 0.000000000000000000, 1.000000000000000000, 0.000000000000000000 ) ) ;
#785 = CARTESIAN_POINT ( 'NONE',  ( 12.13621795668766445, 36.51313500000000545, 4.225309685850866082 ) ) ;
#786 = CARTESIAN_POINT ( 'NONE',  ( 8.850476390893977197, 18.78072660019471840, 6.559035762646428402 ) ) ;
#787 = CARTESIAN_POINT ( 'NONE',  ( 7.228733647532628481, 13.55792429055235715, 6.729328822189224013 ) ) ;
#788 = AXIS2_PLACEMENT_3D ( 'NONE', #5490, #4369, #1956 ) ;
#789 = AXIS2_PLACEMENT_3D ( 'NONE', #10505, #19118, #10616 ) ;
#790 = CARTESIAN_POINT ( 'NONE',  ( 38.23013820809905638, 42.06303499999999929, -14.22485453658974031 ) ) ;
#791 = DIRECTION ( 'NONE',  ( -0.4080888115384288528, 0.000000000000000000, -0.9129422336036122632 ) ) ;
#792 = CARTESIAN_POINT ( 'NONE',  ( 9.070861399739685638, 20.13899192311416186, 6.446725801674014100 ) ) ;
#793 = VECTOR ( 'NONE', #3732, 1000.000000000000114 ) ;
#794 = DIRECTION ( 'NONE',  ( -0.000000000000000000, 1.000000000000000000, 0.000000000000000000 ) ) ;
#795 = CARTESIAN_POINT ( 'NONE',  ( 1.651338490073621879, 16.44735884859098718, -0.7918851340569855735 ) ) ;
#796 = DIRECTION ( 'NONE',  ( 0.000000000000000000, 1.000000000000000000, 0.000000000000000000 ) ) ;
#797 = EDGE_CURVE ( 'NONE', #13084, #13654, #10323, .T. ) ;
#798 = CARTESIAN_POINT ( 'NONE',  ( 6.585898268469219552, 30.56064500000000095, 4.694966092919240275 ) ) ;
#799 = CARTESIAN_POINT ( 'NONE',  ( 2.084092584291341588, 17.94179249953145217, 0.2586688736977448833 ) ) ;
#800 = PLANE ( 'NONE',  #15930 ) ;
#801 = FACE_OUTER_BOUND ( 'NONE', #18130, .T. ) ;
#802 = CARTESIAN_POINT ( 'NONE',  ( 19.23564988699146383, 0.9575902230288153572, -14.49006204532864928 ) ) ;
#803 = ORIENTED_EDGE ( 'NONE', *, *, #7640, .T. ) ;
#804 = DIRECTION ( 'NONE',  ( 0.000000000000000000, 1.000000000000000000, 0.000000000000000000 ) ) ;
#805 = VECTOR ( 'NONE', #14773, 1000.000000000000114 ) ;
#806 = VECTOR ( 'NONE', #16119, 1000.000000000000000 ) ;
#807 = CARTESIAN_POINT ( 'NONE',  ( 11.12436898423977638, 12.00734156490978677, 5.678099997755476025 ) ) ;
#808 = EDGE_LOOP ( 'NONE', ( #8099, #12394, #12847, #19398, #3996, #13078 ) ) ;
#809 = DIRECTION ( 'NONE',  ( 0.000000000000000000, 1.000000000000000000, 0.000000000000000000 ) ) ;
#810 = CARTESIAN_POINT ( 'NONE',  ( 11.59421558736491598, 19.10596872916567435, -2.836117574684339449 ) ) ;
#811 = CARTESIAN_POINT ( 'NONE',  ( 5.370882954727737690, 14.76353563683550263, -1.916208718001963796 ) ) ;
#812 = DIRECTION ( 'NONE',  ( 0.000000000000000000, 1.000000000000000000, 0.000000000000000000 ) ) ;
#813 = CARTESIAN_POINT ( 'NONE',  ( 1.770729414466086782, 14.88544593074506928, 0.2654498043701122301 ) ) ;
#814 = ORIENTED_EDGE ( 'NONE', *, *, #7876, .F. ) ;
#815 = ITEM_DEFINED_TRANSFORMATION ( 'NONE', 'NONE', #3482,  #2234 ) ;
#816 = CARTESIAN_POINT ( 'NONE',  ( -0.1849527129589544072, 21.03045532914853055, 5.150944214860931680 ) ) ;
#817 = AXIS2_PLACEMENT_3D ( 'NONE', #3190, #18327, #3407 ) ;
#818 = CARTESIAN_POINT ( 'NONE',  ( -2.028188046367890074, 9.924415000000001541, 0.3682158094503220069 ) ) ;
#819 = ORIENTED_EDGE ( 'NONE', *, *, #16382, .T. ) ;
#820 = CARTESIAN_POINT ( 'NONE',  ( 6.917893308609325942, 12.02983150285682079, 4.746903262785427735 ) ) ;
#821 = CARTESIAN_POINT ( 'NONE',  ( 9.401342779853303355, 17.21989818313373988, -2.904324505523894651 ) ) ;
#822 = CARTESIAN_POINT ( 'NONE',  ( 10.88895342146457601, 14.15760627606356081, -4.055013420937678248 ) ) ;
#823 = ADVANCED_FACE ( 'NONE', ( #18322 ), #1521, .F. ) ;
#824 = DIRECTION ( 'NONE',  ( -0.1060008583745224581, 0.000000000000000000, -0.9943660382494288186 ) ) ;
#825 = VECTOR ( 'NONE', #16124, 1000.000000000000227 ) ;
#826 = PRODUCT_DEFINITION_CONTEXT ( 'detailed design', #18349, 'design' ) ;
#827 = DIRECTION ( 'NONE',  ( 0.000000000000000000, 1.000000000000000000, 0.000000000000000000 ) ) ;
#828 = ORIENTED_EDGE ( 'NONE', *, *, #12493, .F. ) ;
#829 = CARTESIAN_POINT ( 'NONE',  ( 5.317747445270939011, 13.58815257356176076, -1.516694713297795261 ) ) ;
#830 = CARTESIAN_POINT ( 'NONE',  ( 52.22368883687065022, 39.20681492737163154, -17.56171959381228476 ) ) ;
#831 = VERTEX_POINT ( 'NONE', #12016 ) ;
#832 = CARTESIAN_POINT ( 'NONE',  ( 11.63049744206901792, 21.11709313486170103, 2.852222637699519669 ) ) ;
#833 = CARTESIAN_POINT ( 'NONE',  ( 26.59062499999999929, 2.380615000000000148, 8.731249999999999289 ) ) ;
#834 = CIRCLE ( 'NONE', #8244, 30.16249999999998721 ) ;
#835 = CARTESIAN_POINT ( 'NONE',  ( 0.9037643508957434735, 18.98659669545878259, 7.881339249872772790 ) ) ;
#837 = CARTESIAN_POINT ( 'NONE',  ( 59.52193197173441774, -1.983739999999999837, -3.260183413611184911 ) ) ;
#836 = CARTESIAN_POINT ( 'NONE',  ( 5.211679344434179129, 21.23839086782724195, 3.885610057435962439 ) ) ;
#838 = ORIENTED_EDGE ( 'NONE', *, *, #9399, .T. ) ;
#839 = DIRECTION ( 'NONE',  ( 0.8558687090795832342, 0.000000000000000000, -0.5171931484643309540 ) ) ;
#840 = CARTESIAN_POINT ( 'NONE',  ( 26.59062499999999929, 5.953125000000000000, 10.71562499999999929 ) ) ;
#841 = ORIENTED_EDGE ( 'NONE', *, *, #10075, .F. ) ;
#842 = DIRECTION ( 'NONE',  ( 0.000000000000000000, 1.000000000000000000, 0.000000000000000000 ) ) ;
#843 = EDGE_CURVE ( 'NONE', #5953, #16263, #20185, .T. ) ;
#844 = AXIS2_PLACEMENT_3D ( 'NONE', #8969, #14195, #20909 ) ;
#845 = CARTESIAN_POINT ( 'NONE',  ( 12.49368766438004918, -5.659044190558311094, -16.93738714635493992 ) ) ;
#846 = ORIENTED_EDGE ( 'NONE', *, *, #8565, .F. ) ;
#847 = CARTESIAN_POINT ( 'NONE',  ( 13.67756757867809725, -5.959792500000001603, 2.571257636385987144 ) ) ;
#848 = CARTESIAN_POINT ( 'NONE',  ( -15.27935546639805331, -3.968114999999999615, -26.04713531390440906 ) ) ;
#849 = CARTESIAN_POINT ( 'NONE',  ( 12.06368358668478891, 10.32531656698114020, 0.6252471565032120537 ) ) ;
#850 = ADVANCED_FACE ( 'NONE', ( #10135 ), #72, .T. ) ;
#851 = EDGE_CURVE ( 'NONE', #6512, #12344, #17443, .T. ) ;
#852 = CIRCLE ( 'NONE', #12513, 0.3962399999999990929 ) ;
#853 = CARTESIAN_POINT ( 'NONE',  ( 21.25660046192028929, -3.968114999999999615, -13.18703856829094079 ) ) ;
#854 = EDGE_LOOP ( 'NONE', ( #772, #16081, #18567, #4619, #13382, #13035, #9205, #19390, #3885, #9519, #20998, #18124, #9666, #2739, #11741, #2851, #8488, #10820, #3221, #4979, #18354 ) ) ;
#855 = LINE ( 'NONE', #17779, #102 ) ;
#856 = CARTESIAN_POINT ( 'NONE',  ( 38.94885947252247860, -7.547248457916676756, -3.956611957470116625 ) ) ;
#857 = AXIS2_PLACEMENT_3D ( 'NONE', #12113, #15668, #1410 ) ;
#858 = ORIENTED_EDGE ( 'NONE', *, *, #4636, .F. ) ;
#859 = ORIENTED_EDGE ( 'NONE', *, *, #3535, .T. ) ;
#860 = FACE_OUTER_BOUND ( 'NONE', #15123, .T. ) ;
#862 = FACE_BOUND ( 'NONE', #9935, .T. ) ;
#861 = CARTESIAN_POINT ( 'NONE',  ( 2.098362976749927888, 11.83352507831272149, 1.754813491889370747 ) ) ;
#863 = ORIENTED_EDGE ( 'NONE', *, *, #16462, .T. ) ;
#864 = CARTESIAN_POINT ( 'NONE',  ( 3.589437315726493605, 16.93684646903384206, -1.402224914170865810 ) ) ;
#865 = ORIENTED_EDGE ( 'NONE', *, *, #1285, .F. ) ;
#866 = ORIENTED_EDGE ( 'NONE', *, *, #19505, .T. ) ;
#867 = VECTOR ( 'NONE', #15872, 1000.000000000000000 ) ;
#868 = ADVANCED_FACE ( 'NONE', ( #18966 ), #7371, .T. ) ;
#869 = CARTESIAN_POINT ( 'NONE',  ( 1.435649018927920739, 14.09384548075437138, 8.206564140987731903 ) ) ;
#870 = ORIENTED_EDGE ( 'NONE', *, *, #639, .T. ) ;
#871 = CIRCLE ( 'NONE', #6171, 3.174999999999998490 ) ;
#872 = EDGE_CURVE ( 'NONE', #8553, #5503, #6086, .T. ) ;
#873 = CARTESIAN_POINT ( 'NONE',  ( 11.57071721368057915, 0.2046444788096904999, 9.611460029477360223 ) ) ;
#874 = CARTESIAN_POINT ( 'NONE',  ( 59.55063415577301811, 32.54502000000000095, -22.52230776719629191 ) ) ;
#875 = CARTESIAN_POINT ( 'NONE',  ( 2.492193568723835462, -69.63187750000000165, -24.56873394466936134 ) ) ;
#876 = CARTESIAN_POINT ( 'NONE',  ( 2.788940323695707768, 11.28012997864750311, 4.828948434681314517 ) ) ;
#877 = VERTEX_POINT ( 'NONE', #9239 ) ;
#878 = CARTESIAN_POINT ( 'NONE',  ( 7.672689199289790984, 14.92411314052326965, 7.513769365600475147 ) ) ;
#879 = CARTESIAN_POINT ( 'NONE',  ( -1.427050033073577806, 5.548947500000001476, -23.44038945102687066 ) ) ;
#880 = CARTESIAN_POINT ( 'NONE',  ( 13.28857892897944382, 22.14715058108314594, 1.978915458932410720 ) ) ;
#881 = CYLINDRICAL_SURFACE ( 'NONE', #9261, 1.190624999999997824 ) ;
#882 = EDGE_CURVE ( 'NONE', #20855, #10784, #15692, .T. ) ;
#883 = EDGE_LOOP ( 'NONE', ( #644, #21861, #15270, #2551 ) ) ;
#884 = ORIENTED_EDGE ( 'NONE', *, *, #3946, .T. ) ;
#885 = CARTESIAN_POINT ( 'NONE',  ( 5.451387325446391152, 19.02104356353402181, -1.049876524968703428 ) ) ;
#887 = DIRECTION ( 'NONE',  ( -0.3482992169606098365, 0.9330960544336215357, -0.08955115110948595747 ) ) ;
#886 = CARTESIAN_POINT ( 'NONE',  ( 29.98909767165928386, 39.28268749999999443, -5.214162619065493054 ) ) ;
#888 = CARTESIAN_POINT ( 'NONE',  ( 12.66657608565324544, 10.81635483712285151, 3.529341624401947541 ) ) ;
#889 = ORIENTED_EDGE ( 'NONE', *, *, #967, .T. ) ;
#890 = VECTOR ( 'NONE', #9483, 1000.000000000000000 ) ;
#891 = ORIENTED_EDGE ( 'NONE', *, *, #18599, .F. ) ;
#892 = FACE_OUTER_BOUND ( 'NONE', #17084, .T. ) ;
#893 = CARTESIAN_POINT ( 'NONE',  ( 7.233312877372291894, 16.04677007903879726, -2.879531353839789087 ) ) ;
#894 = DIRECTION ( 'NONE',  ( 0.2868778675745010664, 0.000000000000000000, 0.9579671649362032637 ) ) ;
#895 = CARTESIAN_POINT ( 'NONE',  ( 59.90456643211351917, 37.11476346399999926, -2.926035437812116946 ) ) ;
#896 = EDGE_CURVE ( 'NONE', #10916, #13402, #20547, .T. ) ;
#897 = CARTESIAN_POINT ( 'NONE',  ( 8.104304450262016957, 20.50171273394048299, 4.697722215350715658 ) ) ;
#898 = ADVANCED_FACE ( 'NONE', ( #17208 ), #2170, .T. ) ;
#899 = ADVANCED_FACE ( 'NONE', ( #19304 ), #7270, .T. ) ;
#900 = DIRECTION ( 'NONE',  ( 0.000000000000000000, 1.000000000000000000, 0.000000000000000000 ) ) ;
#901 = CARTESIAN_POINT ( 'NONE',  ( 7.526225150842845046, 18.37388711802374530, -2.690556271596364901 ) ) ;
#902 = CARTESIAN_POINT ( 'NONE',  ( 62.90077106633562209, -1.983739999999999393, 8.141649473166729933 ) ) ;
#903 = CARTESIAN_POINT ( 'NONE',  ( -23.36909032872569014, 3.961447500000001565, -10.47372115209112842 ) ) ;
#904 = CARTESIAN_POINT ( 'NONE',  ( 0.7365175131326759939, 11.31684784372412089, 4.865384749232847916 ) ) ;
#905 = CARTESIAN_POINT ( 'NONE',  ( 0.5885023020491949586, 11.47569386093249300, 4.096986995605308657 ) ) ;
#906 = FACE_OUTER_BOUND ( 'NONE', #1227, .T. ) ;
#907 = CARTESIAN_POINT ( 'NONE',  ( 5.237852948251049412, 17.31877066267591658, 8.028226905314944872 ) ) ;
#908 = CARTESIAN_POINT ( 'NONE',  ( 1.336191582698512681, 23.41816499999998769, 10.66779613908654056 ) ) ;
#909 = DIRECTION ( 'NONE',  ( 0.000000000000000000, -1.000000000000000000, -0.000000000000000000 ) ) ;
#910 = CARTESIAN_POINT ( 'NONE',  ( 12.58231226417771431, 1.068540657403270533, -16.47635048232419308 ) ) ;
#911 = EDGE_LOOP ( 'NONE', ( #2038, #5013, #2441, #3955 ) ) ;
#912 = DIRECTION ( 'NONE',  ( 0.000000000000000000, 1.000000000000000000, 0.000000000000000000 ) ) ;
#913 = CARTESIAN_POINT ( 'NONE',  ( 9.454490738039723396, 11.77944925497319595, -1.426592419569617354 ) ) ;
#914 = EDGE_LOOP ( 'NONE', ( #6101, #19962 ) ) ;
#915 = CARTESIAN_POINT ( 'NONE',  ( 29.35287372532640049, 1.909660849011530104, 10.71464187463071838 ) ) ;
#916 = CARTESIAN_POINT ( 'NONE',  ( 5.487919320111488197, 17.38806467533618516, -2.066457398598804396 ) ) ;
#917 = LINE ( 'NONE', #20928, #8769 ) ;
#918 = CARTESIAN_POINT ( 'NONE',  ( 0.3644238609685282460, 12.38707500932596162, 3.460104896903041016 ) ) ;
#919 = ORIENTED_EDGE ( 'NONE', *, *, #7931, .T. ) ;
#920 = CARTESIAN_POINT ( 'NONE',  ( 12.57635667311951622, -95.96551800000000298, 1.354834321244424267 ) ) ;
#921 = CARTESIAN_POINT ( 'NONE',  ( 5.850959131300735194, 20.65587636292193352, 4.328574444934527143 ) ) ;
#922 = ADVANCED_FACE ( 'NONE', ( #2286 ), #10909, .F. ) ;
#923 = CARTESIAN_POINT ( 'NONE',  ( 53.00421038040393995, 0.000000000000000000, 6.511420152579801446 ) ) ;
#924 = ORIENTED_EDGE ( 'NONE', *, *, #3296, .T. ) ;
#925 = CARTESIAN_POINT ( 'NONE',  ( 9.411590077691956324, 21.23906099414256232, 1.666482855468156332 ) ) ;
#926 = CARTESIAN_POINT ( 'NONE',  ( 9.754543803393604051, 21.05370774754728203, 3.404076865865295343 ) ) ;
#927 = CARTESIAN_POINT ( 'NONE',  ( 3.676745431939328235, 18.24815116393151015, 8.767987032105414968 ) ) ;
#928 = CARTESIAN_POINT ( 'NONE',  ( 13.54273369681055428, 22.20171528482708112, 2.439503800205132134 ) ) ;
#929 = CARTESIAN_POINT ( 'NONE',  ( 53.50176854207381183, -7.446663216667899654, -16.23620094008295567 ) ) ;
#930 = CARTESIAN_POINT ( 'NONE',  ( 39.90410341501912939, 39.21273375806297423, -3.030981210009983329 ) ) ;
#931 = CARTESIAN_POINT ( 'NONE',  ( 3.128535511035963612, 21.16459892206533056, 2.693085165987005869 ) ) ;
#932 = DIRECTION ( 'NONE',  ( 0.9964481331860212121, 0.000000000000000000, -0.08420877549337300871 ) ) ;
#933 = ORIENTED_EDGE ( 'NONE', *, *, #3535, .F. ) ;
#934 = CARTESIAN_POINT ( 'NONE',  ( 52.55824432597118800, 39.85392714130129832, -17.26273071540813930 ) ) ;
#935 = ORIENTED_EDGE ( 'NONE', *, *, #8739, .T. ) ;
#936 = CARTESIAN_POINT ( 'NONE',  ( 10.90457161609252168, 21.16733262328514442, 0.8920809610247827370 ) ) ;
#937 = DIRECTION ( 'NONE',  ( 0.000000000000000000, 0.000000000000000000, 1.000000000000000000 ) ) ;
#938 = CARTESIAN_POINT ( 'NONE',  ( 0.2293556595113930840, 20.07828324242409579, 6.214976256840158975 ) ) ;
#940 = CARTESIAN_POINT ( 'NONE',  ( 38.23013820809905638, 109.3223030719999969, -14.22485453658974031 ) ) ;
#939 = CARTESIAN_POINT ( 'NONE',  ( 2.064884689569050469, 11.61267145053902006, 3.635488099080468327 ) ) ;
#941 = EDGE_LOOP ( 'NONE', ( #20654, #15170, #9199, #19380 ) ) ;
#942 = DIRECTION ( 'NONE',  ( 0.000000000000000000, -1.000000000000000000, 0.000000000000000000 ) ) ;
#943 = EDGE_CURVE ( 'NONE', #17008, #1261, #5484, .T. ) ;
#944 = DIRECTION ( 'NONE',  ( -0.2868778675745011220, 0.000000000000000000, -0.9579671649362034858 ) ) ;
#945 = ORIENTED_EDGE ( 'NONE', *, *, #5714, .F. ) ;
#946 = PLANE ( 'NONE',  #19198 ) ;
#947 = CARTESIAN_POINT ( 'NONE',  ( 14.42288723307214937, 1.091498886294842929, -16.08015919209965361 ) ) ;
#948 = ORIENTED_EDGE ( 'NONE', *, *, #19907, .F. ) ;
#949 = CARTESIAN_POINT ( 'NONE',  ( 12.44452585099119624, 19.94285714604490067, 5.084842939140666651 ) ) ;
#950 = VECTOR ( 'NONE', #4203, 1000.000000000000000 ) ;
#951 = DIRECTION ( 'NONE',  ( 0.08420877549337300871, 0.000000000000000000, 0.9964481331860212121 ) ) ;
#952 = ORIENTED_EDGE ( 'NONE', *, *, #8551, .F. ) ;
#953 = CYLINDRICAL_SURFACE ( 'NONE', #8579, 1.190624999999999822 ) ;
#955 = DIRECTION ( 'NONE',  ( 1.000000000000000000, 0.000000000000000000, 0.000000000000000000 ) ) ;
#954 = DIRECTION ( 'NONE',  ( 0.000000000000000000, 1.000000000000000000, 0.000000000000000000 ) ) ;
#956 = EDGE_LOOP ( 'NONE', ( #8354, #9146, #16354, #4398, #16333 ) ) ;
#957 = ORIENTED_EDGE ( 'NONE', *, *, #13068, .F. ) ;
#958 = CARTESIAN_POINT ( 'NONE',  ( 65.90927232300019512, 32.54502000000000095, -13.30734117861468135 ) ) ;
#960 = PLANE ( 'NONE',  #2143 ) ;
#959 = CARTESIAN_POINT ( 'NONE',  ( -0.07327418442642195939, 17.37668286801814688, 0.02659433903688191228 ) ) ;
#961 = ORIENTED_EDGE ( 'NONE', *, *, #2073, .T. ) ;
#962 = CARTESIAN_POINT ( 'NONE',  ( 3.826978250008152838, 18.56559772987111856, -0.9675601391790299433 ) ) ;
#963 = ORIENTED_EDGE ( 'NONE', *, *, #13424, .F. ) ;
#964 = EDGE_CURVE ( 'NONE', #12607, #1384, #20908, .T. ) ;
#965 = CIRCLE ( 'NONE', #18263, 4.365624999999999645 ) ;
#966 = VERTEX_POINT ( 'NONE', #17658 ) ;
#967 = EDGE_CURVE ( 'NONE', #10206, #3833, #5592, .T. ) ;
#968 = VERTEX_POINT ( 'NONE', #12242 ) ;
#969 = DIRECTION ( 'NONE',  ( 0.2490110332224846623, 0.000000000000000000, -0.9685006480810793850 ) ) ;
#970 = FACE_OUTER_BOUND ( 'NONE', #7558, .T. ) ;
#971 = CARTESIAN_POINT ( 'NONE',  ( 2.063750000000000195, 1.984375000000000000, -16.49278420930464861 ) ) ;
#972 = DIRECTION ( 'NONE',  ( 0.08420877549337300871, 0.000000000000000000, 0.9964481331860212121 ) ) ;
#973 = CARTESIAN_POINT ( 'NONE',  ( 3.099914158177832224, 11.64373280860985105, 6.183033039608584858 ) ) ;
#974 = ORIENTED_EDGE ( 'NONE', *, *, #1086, .T. ) ;
#975 = CARTESIAN_POINT ( 'NONE',  ( -17.46249999999999858, 0.000000000000000000, 0.000000000000000000 ) ) ;
#976 = DIRECTION ( 'NONE',  ( -0.9987059298363656357, 0.000000000000000000, -0.05085730733808393328 ) ) ;
#977 = DIRECTION ( 'NONE',  ( 0.000000000000000000, 1.000000000000000000, 0.000000000000000000 ) ) ;
#978 = CARTESIAN_POINT ( 'NONE',  ( -29.36874999999999858, 2.380615000000000148, 8.731249999999999289 ) ) ;
#979 = EDGE_CURVE ( 'NONE', #12825, #9462, #12474, .T. ) ;
#980 = ORIENTED_EDGE ( 'NONE', *, *, #6673, .F. ) ;
#981 = ORIENTED_EDGE ( 'NONE', *, *, #3143, .F. ) ;
#982 = CARTESIAN_POINT ( 'NONE',  ( 10.60640877659219861, 16.27109148020024421, -3.957100436307429359 ) ) ;
#983 = APPLICATION_CONTEXT ( 'automotive_design' ) ;
#984 = FACE_OUTER_BOUND ( 'NONE', #3236, .T. ) ;
#985 = CARTESIAN_POINT ( 'NONE',  ( 11.62203808576201958, 20.29981520329449296, -2.921068254133583508 ) ) ;
#986 = ORIENTED_EDGE ( 'NONE', *, *, #17962, .F. ) ;
#987 = ORIENTED_EDGE ( 'NONE', *, *, #21537, .F. ) ;
#988 = CARTESIAN_POINT ( 'NONE',  ( 21.25660046192028929, 36.51313500000000545, -13.18703856829094079 ) ) ;
#989 = EDGE_CURVE ( 'NONE', #17468, #15052, #4063, .T. ) ;
#990 = CARTESIAN_POINT ( 'NONE',  ( 7.469192301192234318, 18.32891399945091848, -2.552061295666830265 ) ) ;
#991 = DIRECTION ( 'NONE',  ( 0.000000000000000000, 1.000000000000000000, 0.000000000000000000 ) ) ;
#992 = EDGE_CURVE ( 'NONE', #20634, #7630, #3840, .T. ) ;
#993 = CARTESIAN_POINT ( 'NONE',  ( 8.898720949407623593, 18.59683926628043338, 6.668590119552477269 ) ) ;
#994 = VECTOR ( 'NONE', #12853, 1000.000000000000000 ) ;
#995 = CARTESIAN_POINT ( 'NONE',  ( 2.290308818630598431, 20.10037469023196621, 6.068923932348192274 ) ) ;
#996 = CARTESIAN_POINT ( 'NONE',  ( 24.43309469626978725, 23.18727947754285879, -0.6496488801123181389 ) ) ;
#997 = LINE ( 'NONE', #1322, #15546 ) ;
#998 = CARTESIAN_POINT ( 'NONE',  ( 11.50899041575192783, 13.68104675248728164, 7.058214869108054401 ) ) ;
#999 = CARTESIAN_POINT ( 'NONE',  ( 28.38195592936287781, -6.752907499999998286, -13.81504834214261024 ) ) ;
#1000 = DIRECTION ( 'NONE',  ( -0.000000000000000000, 1.000000000000000000, 0.000000000000000000 ) ) ;
#1001 = DIRECTION ( 'NONE',  ( 0.2490110332224850231, 0.000000000000000000, -0.9685006480810791629 ) ) ;
#1002 = CARTESIAN_POINT ( 'NONE',  ( 4.141897743895355255, 11.26628406262684301, 2.001306006738907683 ) ) ;
#1003 = CARTESIAN_POINT ( 'NONE',  ( 0.8150964148941177712, 11.42577256918107054, 5.083379029272794725 ) ) ;
#1004 = CARTESIAN_POINT ( 'NONE',  ( 2.063750000000000195, 24.21318500000000284, 10.71562499999999929 ) ) ;
#1005 = CARTESIAN_POINT ( 'NONE',  ( 5.353244178343441462, 14.21749487271361190, 7.624480077791540467 ) ) ;
#1006 = LINE ( 'NONE', #14849, #1063 ) ;
#1007 = DIRECTION ( 'NONE',  ( 1.000000000000000000, 0.000000000000000000, 0.000000000000000000 ) ) ;
#1008 = CARTESIAN_POINT ( 'NONE',  ( 20.27534158291089383, -5.683549201221528513, -13.95679996024211178 ) ) ;
#1009 = EDGE_CURVE ( 'NONE', #968, #19531, #14254, .T. ) ;
#1010 = VERTEX_POINT ( 'NONE', #12138 ) ;
#1011 = CARTESIAN_POINT ( 'NONE',  ( 61.65536943582333151, 0.000000000000000000, -11.98363747855214712 ) ) ;
#1012 = PRODUCT_DEFINITION ( 'UNKNOWN', '', #20389, #10115 ) ;
#1013 = VECTOR ( 'NONE', #20361, 1000.000000000000114 ) ;
#1014 = CARTESIAN_POINT ( 'NONE',  ( 11.44223642946347042, 15.42323504901881748, 7.509133475055971729 ) ) ;
#1015 = ORIENTED_EDGE ( 'NONE', *, *, #17671, .F. ) ;
#1016 = CARTESIAN_POINT ( 'NONE',  ( 26.96090640492720425, 1.228048945539309766, 10.56624576331076071 ) ) ;
#1017 = CARTESIAN_POINT ( 'NONE',  ( 11.75036113457564113, 19.64364350978045692, -2.459295084851638613 ) ) ;
#1018 = CARTESIAN_POINT ( 'NONE',  ( 5.438185394540740347, 13.64782653932916112, -1.443462502430749694 ) ) ;
#1019 = DIRECTION ( 'NONE',  ( -0.9966381950048638361, 0.000000000000000000, 0.08192867786951606168 ) ) ;
#1020 = CARTESIAN_POINT ( 'NONE',  ( 5.534656983323768209, 20.82992769506763864, 3.759961556826081353 ) ) ;
#1021 = VERTEX_POINT ( 'NONE', #8792 ) ;
#1022 =( NAMED_UNIT ( * ) SI_UNIT ( $, .STERADIAN. ) SOLID_ANGLE_UNIT ( ) );
#1023 = CARTESIAN_POINT ( 'NONE',  ( 5.724697889559749342, 20.71246359673639148, 3.995336445546636472 ) ) ;
#1024 = LINE ( 'NONE', #4465, #19918 ) ;
#1025 = ORIENTED_EDGE ( 'NONE', *, *, #19522, .F. ) ;
#1026 = CARTESIAN_POINT ( 'NONE',  ( 5.955902939063514090, 17.26127046106770635, -1.587797145480220440 ) ) ;
#1027 = DIRECTION ( 'NONE',  ( 1.000000000000000000, 0.000000000000000000, 0.000000000000000000 ) ) ;
#1028 = DIRECTION ( 'NONE',  ( 0.000000000000000000, -1.000000000000000000, -0.000000000000000000 ) ) ;
#1029 = AXIS2_PLACEMENT_3D ( 'NONE', #3066, #20273, #16870 ) ;
#1030 = DIRECTION ( 'NONE',  ( 0.000000000000000000, -1.000000000000000000, -0.000000000000000000 ) ) ;
#1031 = FACE_OUTER_BOUND ( 'NONE', #17461, .T. ) ;
#1032 = DIRECTION ( 'NONE',  ( 0.000000000000000000, 1.000000000000000000, -0.000000000000000000 ) ) ;
#1033 = EDGE_CURVE ( 'NONE', #1535, #12957, #405, .T. ) ;
#1034 = VECTOR ( 'NONE', #2801, 1000.000000000000114 ) ;
#1035 = EDGE_CURVE ( 'NONE', #21341, #16128, #2915, .T. ) ;
#1036 = DIRECTION ( 'NONE',  ( -0.3482992169606098365, 0.9330960544336215357, -0.08955115110948595747 ) ) ;
#1037 = ORIENTED_EDGE ( 'NONE', *, *, #13043, .F. ) ;
#1038 = DIRECTION ( 'NONE',  ( 0.000000000000000000, -1.000000000000000000, -0.000000000000000000 ) ) ;
#1039 = DIRECTION ( 'NONE',  ( 0.000000000000000000, 1.000000000000000000, 0.000000000000000000 ) ) ;
#1040 = ORIENTED_EDGE ( 'NONE', *, *, #6973, .F. ) ;
#1041 = CARTESIAN_POINT ( 'NONE',  ( 12.03222557419000083, 20.69458624090882992, 3.924755836542371146 ) ) ;
#1042 = CARTESIAN_POINT ( 'NONE',  ( 53.10651001381376091, 37.69740999999999786, -16.70269254552787075 ) ) ;
#1043 = CARTESIAN_POINT ( 'NONE',  ( 1.475850426351400291, 15.62743466753882871, 8.791782170180653111 ) ) ;
#1044 = CARTESIAN_POINT ( 'NONE',  ( 19.83909275568333186, -0.5540471600307961264, -14.82645783518564109 ) ) ;
#1046 = LINE ( 'NONE', #9338, #10598 ) ;
#1045 = CARTESIAN_POINT ( 'NONE',  ( 5.581558841844106666, 11.65935603284404287, 0.7263510631195396750 ) ) ;
#1047 = ORIENTED_EDGE ( 'NONE', *, *, #11652, .T. ) ;
#1048 = LINE ( 'NONE', #21490, #15598 ) ;
#1049 = FACE_OUTER_BOUND ( 'NONE', #12036, .T. ) ;
#1050 = VERTEX_POINT ( 'NONE', #12996 ) ;
#1051 = CIRCLE ( 'NONE', #4594, 0.3962399999999999811 ) ;
#1052 = CARTESIAN_POINT ( 'NONE',  ( 19.96181834009323097, -0.9481503896113792074, -14.83657039408695510 ) ) ;
#1053 = CARTESIAN_POINT ( 'NONE',  ( 0.2174850097829113538, 17.55712011575143450, 0.9574576086920399964 ) ) ;
#1054 = VERTEX_POINT ( 'NONE', #6558 ) ;
#1055 = CARTESIAN_POINT ( 'NONE',  ( 13.10833390419068323, 16.70056792996117068, 6.512416574496136867 ) ) ;
#1056 = CARTESIAN_POINT ( 'NONE',  ( 2.655202054194977457, 19.64359183480943472, 1.537090893787881996 ) ) ;
#1057 = CARTESIAN_POINT ( 'NONE',  ( 13.66015131967467156, 22.20657701893900082, 2.405489038835227689 ) ) ;
#1058 =( GEOMETRIC_REPRESENTATION_CONTEXT ( 3 ) GLOBAL_UNCERTAINTY_ASSIGNED_CONTEXT ( ( #18944 ) ) GLOBAL_UNIT_ASSIGNED_CONTEXT ( ( #20231, #6550, #3348 ) ) REPRESENTATION_CONTEXT ( 'NONE', 'WORKASPACE' ) );
#1059 = CARTESIAN_POINT ( 'NONE',  ( 20.09804786238122887, -3.027183637114436721, -15.33410839348449528 ) ) ;
#1060 = EDGE_CURVE ( 'NONE', #11223, #2583, #1466, .T. ) ;
#1061 = CARTESIAN_POINT ( 'NONE',  ( 70.64340948846358970, 32.54502000000000095, -10.93409647675949969 ) ) ;
#1062 = ORIENTED_EDGE ( 'NONE', *, *, #13513, .T. ) ;
#1063 = VECTOR ( 'NONE', #5977, 1000.000000000000114 ) ;
#1064 = CARTESIAN_POINT ( 'NONE',  ( 22.02657784715807665, 128.5105379999999968, -12.98906981665815330 ) ) ;
#1065 = VECTOR ( 'NONE', #13779, 1000.000000000000000 ) ;
#1066 = PLANE ( 'NONE',  #17926 ) ;
#1067 = ORIENTED_EDGE ( 'NONE', *, *, #1108, .F. ) ;
#1068 = VERTEX_POINT ( 'NONE', #18065 ) ;
#1069 = CARTESIAN_POINT ( 'NONE',  ( 10.37745330590589177, -3.119969851305963271, -17.16587059559704187 ) ) ;
#1071 = DIRECTION ( 'NONE',  ( 0.9685006480810790519, 0.000000000000000000, 0.2490110332224857170 ) ) ;
#1070 = CARTESIAN_POINT ( 'NONE',  ( 1.263612230954551441, 21.11436061630988092, 3.307233376954588078 ) ) ;
#1072 = ORIENTED_EDGE ( 'NONE', *, *, #9091, .F. ) ;
#1073 = CARTESIAN_POINT ( 'NONE',  ( 3.760528279849136180, 12.52252298731752767, 0.1935317675302483942 ) ) ;
#1074 = VERTEX_POINT ( 'NONE', #6656 ) ;
#1075 = AXIS2_PLACEMENT_3D ( 'NONE', #5417, #7209, #5200 ) ;
#1076 = ORIENTED_EDGE ( 'NONE', *, *, #468, .T. ) ;
#1077 = ORIENTED_EDGE ( 'NONE', *, *, #1035, .T. ) ;
#1078 = AXIS2_PLACEMENT_3D ( 'NONE', #1933, #7356, #5576 ) ;
#1079 = AXIS2_PLACEMENT_3D ( 'NONE', #9658, #1255, #20244 ) ;
#1080 = DIRECTION ( 'NONE',  ( -0.7334850928793776870, -0.6768732144311018217, 0.06198604769977172219 ) ) ;
#1081 = CARTESIAN_POINT ( 'NONE',  ( 39.54651519818619221, 37.91656218874415885, -3.347550931093328686 ) ) ;
#1082 = AXIS2_PLACEMENT_3D ( 'NONE', #19728, #13446, #18513 ) ;
#1083 = DIRECTION ( 'NONE',  ( 0.9964481331860213231, 0.000000000000000000, -0.08420877549337293932 ) ) ;
#1084 = CARTESIAN_POINT ( 'NONE',  ( 46.03750000000000142, 32.54502000000000095, -10.31874999999999964 ) ) ;
#1085 = CARTESIAN_POINT ( 'NONE',  ( 3.358315432832535308, 12.36100630735107586, 7.353239250121181847 ) ) ;
#1086 = EDGE_CURVE ( 'NONE', #10374, #6204, #17753, .T. ) ;
#1087 = AXIS2_PLACEMENT_3D ( 'NONE', #11496, #6526, #8379 ) ;
#1088 = ORIENTED_EDGE ( 'NONE', *, *, #10570, .F. ) ;
#1089 = TOROIDAL_SURFACE ( 'NONE', #15240, 3.174999999999999822, 1.190625000000000044 ) ;
#1090 = PLANE ( 'NONE',  #10337 ) ;
#1091 = DIRECTION ( 'NONE',  ( 0.000000000000000000, 1.000000000000000000, 0.000000000000000000 ) ) ;
#1092 = DIRECTION ( 'NONE',  ( 0.9579671649362032637, 0.000000000000000000, -0.2868778675745011775 ) ) ;
#1093 = DIRECTION ( 'NONE',  ( -0.9685006480810791629, 0.000000000000000000, -0.2490110332224850231 ) ) ;
#1094 = FACE_OUTER_BOUND ( 'NONE', #16465, .T. ) ;
#1095 = ORIENTED_EDGE ( 'NONE', *, *, #21176, .F. ) ;
#1096 = VERTEX_POINT ( 'NONE', #4892 ) ;
#1097 = CARTESIAN_POINT ( 'NONE',  ( 9.024438055949596915, 14.85500521735966295, 7.276239533518110036 ) ) ;
#1099 = CARTESIAN_POINT ( 'NONE',  ( 36.80301088673436283, 0.000000000000000000, -23.10021947667301134 ) ) ;
#1098 = CARTESIAN_POINT ( 'NONE',  ( 13.28822531734660828, -3.968114999999999615, -15.23578611614444078 ) ) ;
#1100 = CARTESIAN_POINT ( 'NONE',  ( 10.95655038952506821, 16.44103435568498028, -4.352389034132393419 ) ) ;
#1101 = VERTEX_POINT ( 'NONE', #21702 ) ;
#1102 = CIRCLE ( 'NONE', #15593, 1.785937499999998179 ) ;
#1103 = ORIENTED_EDGE ( 'NONE', *, *, #19401, .T. ) ;
#1104 = DIRECTION ( 'NONE',  ( 0.9579671649362032637, 0.000000000000000000, -0.2868778675745010664 ) ) ;
#1105 = CARTESIAN_POINT ( 'NONE',  ( 8.298824244370219816, 21.01560961795355453, -0.4802659323016266191 ) ) ;
#1106 = CARTESIAN_POINT ( 'NONE',  ( 6.566377038699175550, 20.23523262331454475, 0.6328596530739121206 ) ) ;
#1107 = AXIS2_PLACEMENT_3D ( 'NONE', #8605, #15486, #8489 ) ;
#1108 = EDGE_CURVE ( 'NONE', #9462, #16780, #13415, .T. ) ;
#1109 = AXIS2_PLACEMENT_3D ( 'NONE', #9708, #17905, #16474 ) ;
#1110 = CARTESIAN_POINT ( 'NONE',  ( 13.60230603414709094, 21.45952595875148106, 1.784047991531949817 ) ) ;
#1111 = DIRECTION ( 'NONE',  ( -0.9579671649362032637, 0.000000000000000000, 0.2868778675745010664 ) ) ;
#1112 = DIRECTION ( 'NONE',  ( -0.9129422336036127072, 0.000000000000000000, 0.4080888115384278536 ) ) ;
#1113 = CARTESIAN_POINT ( 'NONE',  ( 2.053946910387165037, 11.83412605131448103, 1.768482334681878765 ) ) ;
#1114 = CARTESIAN_POINT ( 'NONE',  ( 0.5391250270183256532, 11.52139035671227063, 3.880880414641454390 ) ) ;
#1115 = EDGE_CURVE ( 'NONE', #20009, #20529, #13174, .T. ) ;
#1116 = EDGE_CURVE ( 'NONE', #20800, #15003, #18486, .T. ) ;
#1117 = VERTEX_POINT ( 'NONE', #11433 ) ;
#1118 = CARTESIAN_POINT ( 'NONE',  ( 3.546748655274437390, 20.63951482243974311, 3.565519225599600439 ) ) ;
#1119 = DIRECTION ( 'NONE',  ( 0.000000000000000000, -1.000000000000000000, 0.000000000000000000 ) ) ;
#1120 = DIRECTION ( 'NONE',  ( 0.000000000000000000, 0.000000000000000000, 1.000000000000000000 ) ) ;
#1121 = CARTESIAN_POINT ( 'NONE',  ( 20.12232975604240437, -5.942321916599345499, -13.98511480133279150 ) ) ;
#1122 = ORIENTED_EDGE ( 'NONE', *, *, #16792, .F. ) ;
#1123 = DIRECTION ( 'NONE',  ( -0.3928209820863007296, 0.000000000000000000, 0.9196149607486571176 ) ) ;
#1124 = AXIS2_PLACEMENT_3D ( 'NONE', #1554, #6631, #4975 ) ;
#1125 = CARTESIAN_POINT ( 'NONE',  ( 9.071028239221552880, 14.95428965682947364, -3.447124252751109896 ) ) ;
#1126 = VERTEX_POINT ( 'NONE', #8214 ) ;
#1127 = CARTESIAN_POINT ( 'NONE',  ( 28.31895198753520049, 1.479004908355108006, 10.65049700491969986 ) ) ;
#1128 = AXIS2_PLACEMENT_3D ( 'NONE', #3087, #5065, #9811 ) ;
#1129 = CARTESIAN_POINT ( 'NONE',  ( 12.78393319624934676, 21.33321389937485080, 0.2603733278526269568 ) ) ;
#1130 = CARTESIAN_POINT ( 'NONE',  ( 6.221313271974531212, 20.46396301300350373, -0.3603416905545633320 ) ) ;
#1131 = AXIS2_PLACEMENT_3D ( 'NONE', #9158, #5950, #7949 ) ;
#1132 = DIRECTION ( 'NONE',  ( 1.000000000000000000, 0.000000000000000000, 0.000000000000000000 ) ) ;
#1133 = CARTESIAN_POINT ( 'NONE',  ( 0.02879538837996780537, 15.70524387060945948, 0.7619693622286592971 ) ) ;
#1134 = ORIENTED_EDGE ( 'NONE', *, *, #19533, .F. ) ;
#1135 = DIRECTION ( 'NONE',  ( 0.000000000000000000, 1.000000000000000000, 0.000000000000000000 ) ) ;
#1136 = CARTESIAN_POINT ( 'NONE',  ( 39.88301061098722755, 0.000000000000000000, -24.08706006053352411 ) ) ;
#1137 = EDGE_CURVE ( 'NONE', #8133, #7171, #5738, .T. ) ;
#1138 = CIRCLE ( 'NONE', #7141, 4.365625000000000533 ) ;
#1139 = AXIS2_PLACEMENT_3D ( 'NONE', #15940, #16049, #10935 ) ;
#1140 = CYLINDRICAL_SURFACE ( 'NONE', #6685, 22.02656249999999361 ) ;
#1141 = CARTESIAN_POINT ( 'NONE',  ( 9.620285707524375951, 14.85500521735966295, 7.097803873153455179 ) ) ;
#1142 = CARTESIAN_POINT ( 'NONE',  ( 6.016625000000000334, 32.54502000000000095, 2.794000000000000039 ) ) ;
#1143 = CARTESIAN_POINT ( 'NONE',  ( 3.493358086098580895, 18.28455830479323652, 8.910730656749969114 ) ) ;
#1144 = CARTESIAN_POINT ( 'NONE',  ( 45.99559936598748777, 34.52875999999999834, 5.449572532947073000 ) ) ;
#1145 = CIRCLE ( 'NONE', #3270, 6.349999999999999645 ) ;
#1146 = AXIS2_PLACEMENT_3D ( 'NONE', #16018, #14139, #3837 ) ;
#1147 = EDGE_CURVE ( 'NONE', #1819, #7588, #4799, .T. ) ;
#1148 = CARTESIAN_POINT ( 'NONE',  ( 56.47666780297049627, -3.968114999999999615, 1.109116340531466127 ) ) ;
#1149 = CARTESIAN_POINT ( 'NONE',  ( 29.22749461619170219, -6.754812500000002551, -4.986088976786413163 ) ) ;
#1150 = CARTESIAN_POINT ( 'NONE',  ( 28.38195592936287781, 2.770822500000000854, -13.81504834214261024 ) ) ;
#1151 = FACE_OUTER_BOUND ( 'NONE', #18739, .T. ) ;
#1152 = FACE_OUTER_BOUND ( 'NONE', #16617, .T. ) ;
#1153 = VERTEX_POINT ( 'NONE', #3359 ) ;
#1154 = DIRECTION ( 'NONE',  ( -0.8558687090795832342, 0.000000000000000000, 0.5171931484643309540 ) ) ;
#1155 = DIRECTION ( 'NONE',  ( -0.9964481331860213231, 0.000000000000000000, 0.08420877549337311974 ) ) ;
#1156 = VECTOR ( 'NONE', #3402, 1000.000000000000000 ) ;
#1157 = ORIENTED_EDGE ( 'NONE', *, *, #8283, .T. ) ;
#1158 = CARTESIAN_POINT ( 'NONE',  ( 12.44961998140978920, 19.86344286058260877, 5.004692419167065864 ) ) ;
#1159 = CARTESIAN_POINT ( 'NONE',  ( 0.6401730578246815906, 19.56094186154469128, 7.247650664160103062 ) ) ;
#1160 = CARTESIAN_POINT ( 'NONE',  ( 20.35972896993364856, -6.628739050289367718, -15.16768908211401801 ) ) ;
#1161 = DIRECTION ( 'NONE',  ( 0.000000000000000000, 1.000000000000000000, 0.000000000000000000 ) ) ;
#1162 = ORIENTED_EDGE ( 'NONE', *, *, #15592, .F. ) ;
#1163 = CARTESIAN_POINT ( 'NONE',  ( 49.79678389823170903, 34.52875999999999834, -28.13445659451038594 ) ) ;
#1164 = EDGE_LOOP ( 'NONE', ( #7263, #18315, #20283, #12931 ) ) ;
#1165 = CARTESIAN_POINT ( 'NONE',  ( 30.78626241496060700, 30.50833916023545811, -2.552201779827368622 ) ) ;
#1166 = ADVANCED_FACE ( 'NONE', ( #13103 ), #1350, .T. ) ;
#1167 = CARTESIAN_POINT ( 'NONE',  ( 0.1329439002683138471, 16.97859826092474123, 0.8348816815925818036 ) ) ;
#1168 = ADVANCED_FACE ( 'NONE', ( #11530 ), #8094, .T. ) ;
#1169 = EDGE_CURVE ( 'NONE', #1190, #8553, #3129, .T. ) ;
#1170 = CARTESIAN_POINT ( 'NONE',  ( 11.16602196571547800, -3.114676983449079284, -17.69632302812056679 ) ) ;
#1171 = ORIENTED_EDGE ( 'NONE', *, *, #15592, .T. ) ;
#1172 = CARTESIAN_POINT ( 'NONE',  ( 11.27301368098517109, 12.84969026437554085, -2.377990926030757901 ) ) ;
#1173 = CARTESIAN_POINT ( 'NONE',  ( 2.780407218318890816, 19.89006846276929252, 1.848699377103335983 ) ) ;
#1174 = AXIS2_PLACEMENT_3D ( 'NONE', #20913, #5776, #4011 ) ;
#1175 = CARTESIAN_POINT ( 'NONE',  ( 38.76261520251843251, 37.72836252664282597, -4.168749548257426163 ) ) ;
#1176 = CARTESIAN_POINT ( 'NONE',  ( 13.07922436883402639, 18.81117101484460363, 6.777410824046630644 ) ) ;
#1177 = CARTESIAN_POINT ( 'NONE',  ( 20.03340970562774004, -2.288172619315485878, -15.38567779163451910 ) ) ;
#1178 = VECTOR ( 'NONE', #4215, 1000.000000000000000 ) ;
#1179 = ORIENTED_EDGE ( 'NONE', *, *, #6973, .T. ) ;
#1180 = CARTESIAN_POINT ( 'NONE',  ( 15.23205103213198441, 13.08957250000000094, -19.24493258192747902 ) ) ;
#1181 = CARTESIAN_POINT ( 'NONE',  ( 38.82016491058538321, 42.06303499999999929, -14.75770094105646812 ) ) ;
#1182 = ORIENTED_EDGE ( 'NONE', *, *, #6183, .F. ) ;
#1183 = ORIENTED_EDGE ( 'NONE', *, *, #18457, .T. ) ;
#1184 = DIRECTION ( 'NONE',  ( 0.000000000000000000, -1.000000000000000000, -0.000000000000000000 ) ) ;
#1186 = DIRECTION ( 'NONE',  ( 0.000000000000000000, -1.000000000000000000, 0.000000000000000000 ) ) ;
#1185 = CARTESIAN_POINT ( 'NONE',  ( 3.462698832070913113, 13.65298187125114282, -0.7916853570755781888 ) ) ;
#1187 = EDGE_LOOP ( 'NONE', ( #19885, #4119, #17539, #10765 ) ) ;
#1188 = CARTESIAN_POINT ( 'NONE',  ( 4.384153316260242406, 20.40071751837500713, 0.3961553867452964339 ) ) ;
#1189 = CIRCLE ( 'NONE', #7538, 0.3962399999999998701 ) ;
#1190 = VERTEX_POINT ( 'NONE', #3244 ) ;
#1191 = ORIENTED_EDGE ( 'NONE', *, *, #8598, .F. ) ;
#1192 = CARTESIAN_POINT ( 'NONE',  ( 0.7351087584799428365, 12.21554749956470154, 4.727313382918564955 ) ) ;
#1193 = ADVANCED_FACE ( 'NONE', ( #6330 ), #3031, .F. ) ;
#1194 = EDGE_LOOP ( 'NONE', ( #3150, #13135, #19731, #16444 ) ) ;
#1195 = VECTOR ( 'NONE', #7827, 999.9999999999998863 ) ;
#1196 = DIRECTION ( 'NONE',  ( -0.8609107660235849613, 0.000000000000000000, 0.5087559856598092844 ) ) ;
#1197 = CIRCLE ( 'NONE', #13575, 0.7950199999999993938 ) ;
#1198 = CARTESIAN_POINT ( 'NONE',  ( 38.18512253410862201, -6.356984999999999886, -4.927479914652648674 ) ) ;
#1199 = CYLINDRICAL_SURFACE ( 'NONE', #4030, 1.190625000000000488 ) ;
#1200 = DIRECTION ( 'NONE',  ( -0.2490110332224850509, 0.000000000000000000, 0.9685006480810792739 ) ) ;
#1201 = CARTESIAN_POINT ( 'NONE',  ( 3.191654872741395810, 11.85014480429067518, 6.591825004443473190 ) ) ;
#1202 = VERTEX_POINT ( 'NONE', #19816 ) ;
#1203 = DIRECTION ( 'NONE',  ( 0.2672484743474500268, 0.000000000000000000, 0.9636276526537417286 ) ) ;
#1204 = CARTESIAN_POINT ( 'NONE',  ( 26.59062499871549790, 1.984216250000009785, 10.71562498306123956 ) ) ;
#1205 = CARTESIAN_POINT ( 'NONE',  ( 56.47666780297049627, -3.968114999999999615, 1.109116340531466127 ) ) ;
#1206 = DIRECTION ( 'NONE',  ( -0.3542738219355860418, 0.000000000000000000, -0.9351417320872557060 ) ) ;
#1207 = CARTESIAN_POINT ( 'NONE',  ( 53.84912356528904809, 38.73144433068016923, -15.76890250127162219 ) ) ;
#1208 = ORIENTED_EDGE ( 'NONE', *, *, #20286, .F. ) ;
#1209 = VERTEX_POINT ( 'NONE', #4689 ) ;
#1210 = CARTESIAN_POINT ( 'NONE',  ( 10.37976351492118177, 21.20110815220486344, 0.3605273278593796316 ) ) ;
#1212 = DIRECTION ( 'NONE',  ( 1.000000000000000000, 0.000000000000000000, 0.000000000000000000 ) ) ;
#1211 = CARTESIAN_POINT ( 'NONE',  ( 1.317196433845851278, 18.94197024501346505, 8.977327884498558674 ) ) ;
#1213 = AXIS2_PLACEMENT_3D ( 'NONE', #19754, #4306, #16360 ) ;
#1214 = CARTESIAN_POINT ( 'NONE',  ( 11.08703814780444574, 12.78412554608461704, -3.188527895529572831 ) ) ;
#1215 = EDGE_LOOP ( 'NONE', ( #5293, #9550, #511, #6847 ) ) ;
#1216 = VERTEX_POINT ( 'NONE', #20126 ) ;
#1217 = CARTESIAN_POINT ( 'NONE',  ( 32.96560389001691505, 0.000000000000000000, -17.84002872454335886 ) ) ;
#1218 = CARTESIAN_POINT ( 'NONE',  ( 8.120560827974646401, 20.48090210490235918, 4.740215234001606603 ) ) ;
#1219 = CARTESIAN_POINT ( 'NONE',  ( 6.866807723763238336, 12.09672977032890628, 4.952112561794938195 ) ) ;
#1220 = EDGE_CURVE ( 'NONE', #9160, #4533, #11757, .T. ) ;
#1221 = AXIS2_PLACEMENT_3D ( 'NONE', #2364, #9093, #3917 ) ;
#1222 = CARTESIAN_POINT ( 'NONE',  ( 13.47389875389390390, 21.39272917331400947, 1.812698284662595860 ) ) ;
#1223 = CARTESIAN_POINT ( 'NONE',  ( 61.65536943582333151, -1.983739999999999837, -11.98363747855214712 ) ) ;
#1224 = CARTESIAN_POINT ( 'NONE',  ( 3.574308380569269694, 17.35305612800781816, -1.439843021498107278 ) ) ;
#1225 = CARTESIAN_POINT ( 'NONE',  ( 1.555646991996000983, 13.12134795819716615, 8.453438023037161742 ) ) ;
#1226 = DIRECTION ( 'NONE',  ( -0.4987171968201974948, 0.000000000000000000, 0.8667647648559581031 ) ) ;
#1227 = EDGE_LOOP ( 'NONE', ( #9061, #2863, #19485, #6400 ) ) ;
#1228 = CARTESIAN_POINT ( 'NONE',  ( 2.929146897677799011, 12.03771362664550182, 5.053990511100109551 ) ) ;
#1229 = DIRECTION ( 'NONE',  ( 0.000000000000000000, 1.000000000000000000, 0.000000000000000000 ) ) ;
#1230 = LINE ( 'NONE', #7973, #13495 ) ;
#1231 = CARTESIAN_POINT ( 'NONE',  ( 17.36619415103275088, -8.153771590782046275, -14.56055014027420036 ) ) ;
#1232 = CIRCLE ( 'NONE', #9341, 30.16249999999999076 ) ;
#1233 = CARTESIAN_POINT ( 'NONE',  ( 36.80301088673436283, 32.54502000000000095, -23.10021947667301134 ) ) ;
#1234 = ORIENTED_EDGE ( 'NONE', *, *, #7163, .T. ) ;
#1235 = DIRECTION ( 'NONE',  ( -0.2227372614607789347, 0.000000000000000000, -0.9748785115884710528 ) ) ;
#1236 = CARTESIAN_POINT ( 'NONE',  ( 7.111278525918518056, 14.37945976953069227, -2.629222021087245675 ) ) ;
#1237 = CARTESIAN_POINT ( 'NONE',  ( 9.795690773676662744, 20.30269022822975344, -2.134972486994283436 ) ) ;
#1238 = VERTEX_POINT ( 'NONE', #1148 ) ;
#1239 = DIRECTION ( 'NONE',  ( -0.7776383362760926898, 0.000000000000000000, 0.6287118719681938916 ) ) ;
#1240 = CARTESIAN_POINT ( 'NONE',  ( 7.909502645964201051, 21.52839833913197154, 4.227392646788147523 ) ) ;
#1241 = DIRECTION ( 'NONE',  ( 0.4987171968201974948, 0.000000000000000000, -0.8667647648559581031 ) ) ;
#1242 = CARTESIAN_POINT ( 'NONE',  ( 0.4274521096678008947, 18.57721708583670761, 1.304126942807774192 ) ) ;
#1243 = DIRECTION ( 'NONE',  ( 1.000000000000000000, 0.000000000000000000, 0.000000000000000000 ) ) ;
#1244 = EDGE_CURVE ( 'NONE', #3969, #9951, #4333, .T. ) ;
#1245 = ADVANCED_FACE ( 'NONE', ( #4575 ), #11315, .T. ) ;
#1246 = CARTESIAN_POINT ( 'NONE',  ( 11.56192577415882816, 36.51313500000000545, 4.677561850332325299 ) ) ;
#1247 = DIRECTION ( 'NONE',  ( 0.7532174416907910786, 0.000000000000000000, 0.6577716059034319773 ) ) ;
#1248 = CARTESIAN_POINT ( 'NONE',  ( 6.091961158834851453, 12.63305981940006184, 0.05014679470045566023 ) ) ;
#1249 = DIRECTION ( 'NONE',  ( 0.000000000000000000, 1.000000000000000000, 0.000000000000000000 ) ) ;
#1250 = CARTESIAN_POINT ( 'NONE',  ( 4.364534777017994749, 21.23176840745776062, 5.146678813630421345 ) ) ;
#1251 = CARTESIAN_POINT ( 'NONE',  ( 35.15748561355322011, -1.983739999999999837, 0.3244898641346534163 ) ) ;
#1252 = CARTESIAN_POINT ( 'NONE',  ( -3.929154139288399961, 22.62314500000000095, 0.9374890779182719625 ) ) ;
#1253 = CARTESIAN_POINT ( 'NONE',  ( 6.502656462190326003, 11.69884544686561156, 2.814585947965546175 ) ) ;
#1254 = CARTESIAN_POINT ( 'NONE',  ( 39.22869158989735894, 40.05999463121278836, -3.656238088543281695 ) ) ;
#1255 = DIRECTION ( 'NONE',  ( 0.000000000000000000, -1.000000000000000000, 0.000000000000000000 ) ) ;
#1256 = EDGE_LOOP ( 'NONE', ( #8055, #5991, #15134, #11048, #17890, #4299 ) ) ;
#1257 = CYLINDRICAL_SURFACE ( 'NONE', #20191, 5.357812499999999645 ) ;
#1258 = EDGE_CURVE ( 'NONE', #8259, #8918, #16003, .T. ) ;
#1259 = FACE_OUTER_BOUND ( 'NONE', #19368, .T. ) ;
#1260 = AXIS2_PLACEMENT_3D ( 'NONE', #13322, #14664, #16739 ) ;
#1261 = VERTEX_POINT ( 'NONE', #10524 ) ;
#1262 = CARTESIAN_POINT ( 'NONE',  ( 12.08903476211492567, 20.60414639161901107, 4.074121722111526900 ) ) ;
#1263 = DIRECTION ( 'NONE',  ( -0.6702301885068630005, 0.000000000000000000, -0.7421532822901579785 ) ) ;
#1264 = CARTESIAN_POINT ( 'NONE',  ( 19.90082682264116087, -1.596441870638235727, -15.30843464744698501 ) ) ;
#1265 = PLANE ( 'NONE',  #7770 ) ;
#1266 = VERTEX_POINT ( 'NONE', #12086 ) ;
#1267 =( NAMED_UNIT ( * ) PLANE_ANGLE_UNIT ( ) SI_UNIT ( $, .RADIAN. ) );
#1268 = DIRECTION ( 'NONE',  ( -0.1878280753562736327, -0.000000000000000000, -0.9822019212503905194 ) ) ;
#1269 = CARTESIAN_POINT ( 'NONE',  ( 3.855576660607481276, 17.17015518278662611, -0.5977695734878597511 ) ) ;
#1270 = ORIENTED_EDGE ( 'NONE', *, *, #10185, .T. ) ;
#1271 = EDGE_CURVE ( 'NONE', #1509, #15569, #7226, .T. ) ;
#1272 = CARTESIAN_POINT ( 'NONE',  ( 20.22951472560300346, -1.344520626714845069, -14.75553331646387711 ) ) ;
#1273 = CARTESIAN_POINT ( 'NONE',  ( 11.59908291261232094, -3.110513798225231330, -17.38546622976265255 ) ) ;
#1274 = ORIENTED_EDGE ( 'NONE', *, *, #7778, .T. ) ;
#1275 = CARTESIAN_POINT ( 'NONE',  ( 6.918379510864386184, 20.81512969834162163, 1.623812571277526873 ) ) ;
#1276 = CARTESIAN_POINT ( 'NONE',  ( 2.230131626902869701, 18.39186932040918521, 0.5436086090886416144 ) ) ;
#1277 = ADVANCED_FACE ( 'NONE', ( #20683 ), #18810, .T. ) ;
#1278 = CARTESIAN_POINT ( 'NONE',  ( 38.22590828043067290, 38.73299043104906758, -4.868551855887884194 ) ) ;
#1279 = CARTESIAN_POINT ( 'NONE',  ( 5.437298796767638720, 17.41108386104152572, -2.170668680170849463 ) ) ;
#1280 =( REPRESENTATION_RELATIONSHIP ('NONE','NONE', #15554, #11147 ) REPRESENTATION_RELATIONSHIP_WITH_TRANSFORMATION ( #815 )SHAPE_REPRESENTATION_RELATIONSHIP( ) );
#1281 = CARTESIAN_POINT ( 'NONE',  ( -6.268352501604232963, 33.79463943363963807, -35.49402737582801848 ) ) ;
#1282 = DIRECTION ( 'NONE',  ( -0.5087559856598092844, 0.000000000000000000, -0.8609107660235849613 ) ) ;
#1283 = ORIENTED_EDGE ( 'NONE', *, *, #9674, .T. ) ;
#1284 = FACE_OUTER_BOUND ( 'NONE', #12717, .T. ) ;
#1285 = EDGE_CURVE ( 'NONE', #736, #11912, #12594, .T. ) ;
#1286 = CARTESIAN_POINT ( 'NONE',  ( 21.03437500000000071, 30.56064500000000095, 5.159374999999999822 ) ) ;
#1287 = ORIENTED_EDGE ( 'NONE', *, *, #8664, .T. ) ;
#1288 = EDGE_CURVE ( 'NONE', #2524, #17693, #18696, .T. ) ;
#1289 = ORIENTED_EDGE ( 'NONE', *, *, #16141, .F. ) ;
#1290 = ADVANCED_FACE ( 'NONE', ( #17049 ), #1896, .T. ) ;
#1291 = CARTESIAN_POINT ( 'NONE',  ( 21.56164019270388721, -3.402113909207450604, -14.89232589754399072 ) ) ;
#1292 = CARTESIAN_POINT ( 'NONE',  ( 7.043391965848642577, 11.65531656196440125, 6.036309832577432033 ) ) ;
#1293 = ORIENTED_EDGE ( 'NONE', *, *, #4679, .T. ) ;
#1294 = CARTESIAN_POINT ( 'NONE',  ( 3.920931115142209045, 11.91735779063842671, 0.9340496824192962011 ) ) ;
#1295 = VERTEX_POINT ( 'NONE', #13752 ) ;
#1296 = ORIENTED_EDGE ( 'NONE', *, *, #11249, .T. ) ;
#1297 = CIRCLE ( 'NONE', #8709, 9.524999999999996803 ) ;
#1298 = VERTEX_POINT ( 'NONE', #20448 ) ;
#1299 = LINE ( 'NONE', #4515, #19490 ) ;
#1300 = CARTESIAN_POINT ( 'NONE',  ( 3.360635606688116894, -14.84248999999999974, -20.45316710734507026 ) ) ;
#1301 = PLANE ( 'NONE',  #11805 ) ;
#1302 = CARTESIAN_POINT ( 'NONE',  ( 71.03963378001139972, 32.54502000000000095, -10.54138470677948014 ) ) ;
#1303 = CARTESIAN_POINT ( 'NONE',  ( 2.509320924895964477, 11.29223014825765148, 3.623872359968939083 ) ) ;
#1304 = ORIENTED_EDGE ( 'NONE', *, *, #18290, .T. ) ;
#1305 = CARTESIAN_POINT ( 'NONE',  ( 13.67756757867809725, 0.001587500000000546807, 2.571257636385987144 ) ) ;
#1306 = CARTESIAN_POINT ( 'NONE',  ( 46.03750000000000142, 0.000000000000000000, -10.31874999999999964 ) ) ;
#1307 = CARTESIAN_POINT ( 'NONE',  ( 201.9384738932629944, 1.984375000000000000, 10.71562489836746046 ) ) ;
#1308 = EDGE_CURVE ( 'NONE', #13225, #13084, #14235, .T. ) ;
#1309 = CARTESIAN_POINT ( 'NONE',  ( 44.28293121686854761, -14.84248999999999974, -31.08068102505560759 ) ) ;
#1310 = ORIENTED_EDGE ( 'NONE', *, *, #6278, .F. ) ;
#1311 = EDGE_CURVE ( 'NONE', #7810, #19275, #7545, .T. ) ;
#1312 = ORIENTED_EDGE ( 'NONE', *, *, #21259, .T. ) ;
#1313 = CARTESIAN_POINT ( 'NONE',  ( 10.73407978594872247, 12.55266643930576187, 5.489046158664341313 ) ) ;
#1314 = VECTOR ( 'NONE', #9026, 1000.000000000000000 ) ;
#1315 = CARTESIAN_POINT ( 'NONE',  ( 64.19677489640052670, 32.54502000000000095, -11.74367670905533423 ) ) ;
#1316 = CARTESIAN_POINT ( 'NONE',  ( 11.16079976075009306, 18.33999801989851264, -4.031859812358146833 ) ) ;
#1317 = ORIENTED_EDGE ( 'NONE', *, *, #20399, .T. ) ;
#1318 = EDGE_LOOP ( 'NONE', ( #8163, #16401, #5359, #8233 ) ) ;
#1319 = DIRECTION ( 'NONE',  ( 0.2868778675745004558, 0.000000000000000000, 0.9579671649362035968 ) ) ;
#1320 = CARTESIAN_POINT ( 'NONE',  ( 8.614852540573018302, 11.67329553713541301, 3.681175664236859824 ) ) ;
#1321 = CARTESIAN_POINT ( 'NONE',  ( 6.979112806929661517, 12.38239436642183655, 5.473019091119168955 ) ) ;
#1322 = CARTESIAN_POINT ( 'NONE',  ( 66.79943102505561114, 34.52875999999999834, -12.07331878313145168 ) ) ;
#1323 = AXIS2_PLACEMENT_3D ( 'NONE', #10611, #20419, #3763 ) ;
#1324 = DIRECTION ( 'NONE',  ( -0.3447671952293630548, 0.000000000000000000, -0.9386882235831439658 ) ) ;
#1325 = DIRECTION ( 'NONE',  ( 0.000000000000000000, -1.000000000000000000, -0.000000000000000000 ) ) ;
#1326 = CARTESIAN_POINT ( 'NONE',  ( 7.248826198693623546, 18.51489551114278953, 8.068672937415568569 ) ) ;
#1327 = CARTESIAN_POINT ( 'NONE',  ( 1.693473566456777268, 15.76551524387820358, 9.579563128626743307 ) ) ;
#1328 = CARTESIAN_POINT ( 'NONE',  ( 30.02465935949302533, 30.50833916023545811, -2.324128137548288731 ) ) ;
#1329 = VERTEX_POINT ( 'NONE', #6092 ) ;
#1330 = CARTESIAN_POINT ( 'NONE',  ( 1.185359635733331807, 18.49730447209151762, 8.305304426369882975 ) ) ;
#1331 = CARTESIAN_POINT ( 'NONE',  ( 1.603561069792159621, 23.48871702854725996, 10.70056859876313382 ) ) ;
#1332 = FACE_OUTER_BOUND ( 'NONE', #2278, .T. ) ;
#1333 = CARTESIAN_POINT ( 'NONE',  ( 12.18257168130173085, -7.051347156841528907, -15.68602168311090317 ) ) ;
#1334 = CARTESIAN_POINT ( 'NONE',  ( 11.82678039945931481, 34.52875999999999834, -12.74436900065013667 ) ) ;
#1335 = ORIENTED_EDGE ( 'NONE', *, *, #3563, .F. ) ;
#1336 = ADVANCED_FACE ( 'NONE', ( #17716 ), #15964, .T. ) ;
#1337 = CARTESIAN_POINT ( 'NONE',  ( 10.22080760973594060, 10.44972119249194087, 2.230886230584283147 ) ) ;
#1338 = CARTESIAN_POINT ( 'NONE',  ( 9.252248000141340967, 12.72407294680628809, -2.360866086177806356 ) ) ;
#1339 = ORIENTED_EDGE ( 'NONE', *, *, #14024, .F. ) ;
#1340 = AXIS2_PLACEMENT_3D ( 'NONE', #2556, #12406, #17593 ) ;
#1341 = CARTESIAN_POINT ( 'NONE',  ( 6.443349162879769665, 20.91163864500137137, 0.2251968743725665245 ) ) ;
#1342 = CARTESIAN_POINT ( 'NONE',  ( 53.25483508941461963, -9.531985000000000596, -5.879799058943532941 ) ) ;
#1343 = CARTESIAN_POINT ( 'NONE',  ( 2.856790208578295687, 12.03350028468612010, 5.076489826180115905 ) ) ;
#1344 = FACE_OUTER_BOUND ( 'NONE', #19634, .T. ) ;
#1345 = CARTESIAN_POINT ( 'NONE',  ( 11.00242668500211707, 11.56703545653052068, 3.822456357127572257 ) ) ;
#1346 = DIRECTION ( 'NONE',  ( 0.000000000000000000, -1.000000000000000000, 0.000000000000000000 ) ) ;
#1347 = CARTESIAN_POINT ( 'NONE',  ( 4.466030190238354791, 11.34862606615942227, 1.934780985301236322 ) ) ;
#1348 = DIRECTION ( 'NONE',  ( 0.2868778675745011220, 0.000000000000000000, 0.9579671649362034858 ) ) ;
#1349 = AXIS2_PLACEMENT_3D ( 'NONE', #35, #13658, #3583 ) ;
#1350 = CYLINDRICAL_SURFACE ( 'NONE', #3619, 0.5079999999999965654 ) ;
#1351 = CARTESIAN_POINT ( 'NONE',  ( 6.703689575097724784, 11.54993908224053278, 2.743509046784338601 ) ) ;
#1352 = PLANE ( 'NONE',  #4444 ) ;
#1353 = LINE ( 'NONE', #21593, #9596 ) ;
#1354 = LINE ( 'NONE', #4474, #2136 ) ;
#1355 = EDGE_CURVE ( 'NONE', #13546, #14729, #6108, .T. ) ;
#1356 = VERTEX_POINT ( 'NONE', #2346 ) ;
#1357 = CARTESIAN_POINT ( 'NONE',  ( 61.60152099976809126, -1.983739999999999837, -12.48877542598203405 ) ) ;
#1358 = CARTESIAN_POINT ( 'NONE',  ( 64.66604708500285881, -1.983739999999999837, -11.54913207920052720 ) ) ;
#1359 = AXIS2_PLACEMENT_3D ( 'NONE', #18822, #254, #8753 ) ;
#1360 = ORIENTED_EDGE ( 'NONE', *, *, #4217, .F. ) ;
#1361 = CARTESIAN_POINT ( 'NONE',  ( 13.15469369770092989, 14.51428635076888796, 6.086221178321558511 ) ) ;
#1362 = CARTESIAN_POINT ( 'NONE',  ( 61.56621290189396944, 34.52875999999999834, -0.7977859469341201937 ) ) ;
#1363 = CARTESIAN_POINT ( 'NONE',  ( 52.55890053324426248, 37.92160077886185121, -17.26210851293683390 ) ) ;
#1364 = CARTESIAN_POINT ( 'NONE',  ( 12.49611771652354975, -6.111721726754139716, -15.44633277492886592 ) ) ;
#1366 = CARTESIAN_POINT ( 'NONE',  ( 13.37471192292826139, 17.58265891940030556, -17.38954468002155451 ) ) ;
#1365 = CARTESIAN_POINT ( 'NONE',  ( 7.040796410886670742, 14.83344068326428022, 8.020876762884475042 ) ) ;
#1367 = ORIENTED_EDGE ( 'NONE', *, *, #16026, .F. ) ;
#1368 = CARTESIAN_POINT ( 'NONE',  ( 0.000000000000000000, 0.000000000000000000, 0.000000000000000000 ) ) ;
#1369 = DIRECTION ( 'NONE',  ( -0.9822019212503904084, 0.000000000000000000, 0.1878280753562735772 ) ) ;
#1370 = CARTESIAN_POINT ( 'NONE',  ( 42.79471501377724252, 34.52875999999999834, 5.049205022181460834 ) ) ;
#1371 = AXIS2_PLACEMENT_3D ( 'NONE', #14359, #9464, #21074 ) ;
#1372 = ORIENTED_EDGE ( 'NONE', *, *, #1935, .T. ) ;
#1373 = CARTESIAN_POINT ( 'NONE',  ( 20.12904150882413035, -1.237462911438615754, -14.78438767367360285 ) ) ;
#1374 = CARTESIAN_POINT ( 'NONE',  ( 0.1597621683595935593, 17.17245058820156700, 0.8711918762187601528 ) ) ;
#1375 = VERTEX_POINT ( 'NONE', #7425 ) ;
#1376 = CARTESIAN_POINT ( 'NONE',  ( 6.453281463188345946, 11.60683490608310109, 3.227001759829918548 ) ) ;
#1377 = ADVANCED_FACE ( 'NONE', ( #19255 ), #5657, .F. ) ;
#1378 = CIRCLE ( 'NONE', #4216, 0.3962399999999988154 ) ;
#1379 = FACE_OUTER_BOUND ( 'NONE', #20204, .T. ) ;
#1380 = CARTESIAN_POINT ( 'NONE',  ( 13.24595452700000919, 12.74059347184058133, 6.150563788764593198 ) ) ;
#1381 = ADVANCED_BREP_SHAPE_REPRESENTATION ( '', ( #20809, #2234 ), #4182 ) ;
#1382 =( NAMED_UNIT ( * ) PLANE_ANGLE_UNIT ( ) SI_UNIT ( $, .RADIAN. ) );
#1383 = ADVANCED_FACE ( 'NONE', ( #906 ), #2456, .F. ) ;
#1384 = VERTEX_POINT ( 'NONE', #2567 ) ;
#1385 = ADVANCED_FACE ( 'NONE', ( #4114 ), #10856, .F. ) ;
#1386 = ADVANCED_FACE ( 'NONE', ( #17394 ), #7323, .T. ) ;
#1387 = CARTESIAN_POINT ( 'NONE',  ( 8.066674694811821311, 19.54961979818703099, -0.9699248743207408152 ) ) ;
#1388 = CARTESIAN_POINT ( 'NONE',  ( 5.686630817712229558, 12.08264022589296260, -0.3164579326137271775 ) ) ;
#1389 = CARTESIAN_POINT ( 'NONE',  ( 46.03750000000000142, 0.000000000000000000, -10.31874999999999964 ) ) ;
#1390 = EDGE_LOOP ( 'NONE', ( #12121, #4724, #2657, #7632, #2322 ) ) ;
#1391 = ORIENTED_EDGE ( 'NONE', *, *, #17921, .T. ) ;
#1392 = CARTESIAN_POINT ( 'NONE',  ( 20.56513292926062775, -14.84248999999999974, -10.49765270116350280 ) ) ;
#1394 = CARTESIAN_POINT ( 'NONE',  ( 55.56250000000000000, 30.56064500000000095, -10.31874999999999964 ) ) ;
#1393 = CARTESIAN_POINT ( 'NONE',  ( 1.592392888938656714, 13.91834099111223111, 9.138786557039964009 ) ) ;
#1395 = ORIENTED_EDGE ( 'NONE', *, *, #4129, .T. ) ;
#1396 = CARTESIAN_POINT ( 'NONE',  ( 4.775750319492399143, 21.07304345130302181, 1.432334575049791781 ) ) ;
#1397 = CIRCLE ( 'NONE', #21171, 0.7950200000000000600 ) ;
#1398 = ORIENTED_EDGE ( 'NONE', *, *, #18691, .F. ) ;
#1399 = ORIENTED_EDGE ( 'NONE', *, *, #12967, .T. ) ;
#1400 = CIRCLE ( 'NONE', #10270, 0.5080000000000016724 ) ;
#1401 = DIRECTION ( 'NONE',  ( 0.000000000000000000, -1.000000000000000000, 0.000000000000000000 ) ) ;
#1402 = VERTEX_POINT ( 'NONE', #798 ) ;
#1403 = CARTESIAN_POINT ( 'NONE',  ( 2.254736932229037816, 12.49607832033696297, 2.404643631543990967 ) ) ;
#1404 = EDGE_CURVE ( 'NONE', #5048, #5980, #5871, .T. ) ;
#1405 = CARTESIAN_POINT ( 'NONE',  ( 9.504781684163363664, 11.74348662527086162, -1.607088501048118845 ) ) ;
#1406 = PRODUCT_RELATED_PRODUCT_CATEGORY ( 'part', '', ( #19193 ) ) ;
#1407 = VECTOR ( 'NONE', #1001, 1000.000000000000114 ) ;
#1408 = CARTESIAN_POINT ( 'NONE',  ( 12.76235139282079167, 21.25996874134203907, -20.69948241803004407 ) ) ;
#1409 = AXIS2_PLACEMENT_3D ( 'NONE', #14333, #21049, #10673 ) ;
#1410 = DIRECTION ( 'NONE',  ( 1.000000000000000000, 0.000000000000000000, 0.000000000000000000 ) ) ;
#1411 = CARTESIAN_POINT ( 'NONE',  ( 46.07940063401251507, 0.000000000000000000, -26.08707253294707229 ) ) ;
#1412 = CARTESIAN_POINT ( 'NONE',  ( 2.113164745155809321, 19.10603123094681521, 0.07079837725019544337 ) ) ;
#1413 = EDGE_CURVE ( 'NONE', #10320, #7268, #19359, .T. ) ;
#1414 = ORIENTED_EDGE ( 'NONE', *, *, #9671, .F. ) ;
#1415 = EDGE_CURVE ( 'NONE', #7335, #3338, #5734, .T. ) ;
#1416 = LINE ( 'NONE', #8050, #20933 ) ;
#1417 = CARTESIAN_POINT ( 'NONE',  ( 46.03750000000000142, 30.56064500000000095, -10.31874999999999964 ) ) ;
#1418 = FACE_OUTER_BOUND ( 'NONE', #9038, .T. ) ;
#1419 = CARTESIAN_POINT ( 'NONE',  ( 53.57639120092643736, 39.84016936695267930, -16.14136963297940497 ) ) ;
#1420 = ORIENTED_EDGE ( 'NONE', *, *, #5878, .F. ) ;
#1421 = ORIENTED_EDGE ( 'NONE', *, *, #14670, .T. ) ;
#1422 = CARTESIAN_POINT ( 'NONE',  ( 12.86189321301863409, 16.70784808449734982, 6.676389785412363054 ) ) ;
#1423 = CIRCLE ( 'NONE', #8464, 0.5953125000000000222 ) ;
#1424 = CARTESIAN_POINT ( 'NONE',  ( 67.40134256979101224, 32.54502000000000095, -13.30734117861468135 ) ) ;
#1425 = VERTEX_POINT ( 'NONE', #19582 ) ;
#1426 = EDGE_LOOP ( 'NONE', ( #6037, #3965, #6020, #16638 ) ) ;
#1427 = CARTESIAN_POINT ( 'NONE',  ( 26.59062499999999929, 5.953125000000000000, 8.731249999999999289 ) ) ;
#1428 = AXIS2_PLACEMENT_3D ( 'NONE', #20915, #20685, #5542 ) ;
#1429 = CARTESIAN_POINT ( 'NONE',  ( 9.146367685053196084, 13.29999752303458749, 6.171800590334175496 ) ) ;
#1430 = EDGE_CURVE ( 'NONE', #12951, #877, #19467, .T. ) ;
#1431 = ADVANCED_FACE ( 'NONE', ( #7647 ), #14408, .T. ) ;
#1432 = EDGE_CURVE ( 'NONE', #6164, #7181, #16178, .T. ) ;
#1433 = VECTOR ( 'NONE', #5276, 1000.000000000000000 ) ;
#1434 = VECTOR ( 'NONE', #1830, 1000.000000000000114 ) ;
#1435 = DIRECTION ( 'NONE',  ( -0.7421532822901579785, 0.000000000000000000, 0.6702301885068630005 ) ) ;
#1436 = CARTESIAN_POINT ( 'NONE',  ( 9.275488759993784527, 39.28205249999999893, -20.77642327197297689 ) ) ;
#1437 = CARTESIAN_POINT ( 'NONE',  ( 0.02739341652945818245, 12.76637012722054187, 1.557401313085817529 ) ) ;
#1438 = DIRECTION ( 'NONE',  ( -0.3393000355767771259, 0.000000000000000000, 0.9406782052634140578 ) ) ;
#1439 = ORIENTED_EDGE ( 'NONE', *, *, #1863, .T. ) ;
#1440 = CARTESIAN_POINT ( 'NONE',  ( 1.937017454913535719, 20.47856574081302128, 4.897271291058011400 ) ) ;
#1441 = DIRECTION ( 'NONE',  ( 0.9966381950048638361, 0.000000000000000000, -0.08192867786951699149 ) ) ;
#1442 = CARTESIAN_POINT ( 'NONE',  ( 11.97174136233939556, 21.25996874134203551, -17.62449286037261942 ) ) ;
#1443 = CARTESIAN_POINT ( 'NONE',  ( 15.38918027679277856, -8.419993694669582140, -14.99388312876912721 ) ) ;
#1444 = CARTESIAN_POINT ( 'NONE',  ( 12.13621795668766445, -3.968114999999999615, 4.225309685850866082 ) ) ;
#1445 = EDGE_LOOP ( 'NONE', ( #18109, #19711, #10943, #9247 ) ) ;
#1446 = CARTESIAN_POINT ( 'NONE',  ( 5.568602949700707683, 12.07884102837326168, -0.2844809541441045697 ) ) ;
#1447 = CARTESIAN_POINT ( 'NONE',  ( -51.84716326864270286, -5.714364999999999029, -70.46824097531958842 ) ) ;
#1448 = CARTESIAN_POINT ( 'NONE',  ( 9.069221020798989841, 15.12857177743934933, -3.487417871451969464 ) ) ;
#1449 = VERTEX_POINT ( 'NONE', #21235 ) ;
#1450 = MECHANICAL_DESIGN_GEOMETRIC_PRESENTATION_REPRESENTATION (  '', ( #2514 ), #7809 ) ;
#1451 = VECTOR ( 'NONE', #4832, 1000.000000000000000 ) ;
#1452 = CARTESIAN_POINT ( 'NONE',  ( 9.127199320685813078, 18.85452980171875126, 7.399920140601325080 ) ) ;
#1453 = LINE ( 'NONE', #21355, #13072 ) ;
#1454 = CARTESIAN_POINT ( 'NONE',  ( 0.05507860973824520862, 14.29202264928412092, 1.244272104700797410 ) ) ;
#1455 = AXIS2_PLACEMENT_3D ( 'NONE', #16323, #11654, #19616 ) ;
#1456 = DIRECTION ( 'NONE',  ( 0.7421532822901579785, 0.000000000000000000, -0.6702301885068630005 ) ) ;
#1457 = CARTESIAN_POINT ( 'NONE',  ( 7.008079519739982111, 18.28595648477671887, 7.207522408034829020 ) ) ;
#1458 = DIRECTION ( 'NONE',  ( 0.2868778675745011220, 0.000000000000000000, 0.9579671649362033747 ) ) ;
#1459 = AXIS2_PLACEMENT_3D ( 'NONE', #6311, #9520, #1123 ) ;
#1460 = EDGE_CURVE ( 'NONE', #20489, #19935, #16020, .T. ) ;
#1461 = CARTESIAN_POINT ( 'NONE',  ( 11.77775824504519520, 15.70746112734460986, 7.146079882600543165 ) ) ;
#1462 = CARTESIAN_POINT ( 'NONE',  ( 2.596796854730198056, 19.75183458472020348, 0.4273034937204048256 ) ) ;
#1463 = CARTESIAN_POINT ( 'NONE',  ( 52.79771328282338771, 0.000000000000000000, 3.317700572842066986 ) ) ;
#1464 = AXIS2_PLACEMENT_3D ( 'NONE', #18570, #6861, #6961 ) ;
#1465 = AXIS2_PLACEMENT_3D ( 'NONE', #8510, #8080, #8195 ) ;
#1466 = LINE ( 'NONE', #6450, #2210 ) ;
#1467 = LINE ( 'NONE', #7779, #17824 ) ;
#1468 = DIRECTION ( 'NONE',  ( 0.2490110332224846623, 0.000000000000000000, -0.9685006480810793850 ) ) ;
#1469 = CARTESIAN_POINT ( 'NONE',  ( -2.256261688646920227, 9.924415000000001541, -0.3933872460174320240 ) ) ;
#1470 = CARTESIAN_POINT ( 'NONE',  ( 54.55586098912687731, 42.06303499999999929, -6.056925149195119040 ) ) ;
#1471 = AXIS2_PLACEMENT_3D ( 'NONE', #4974, #20002, #14962 ) ;
#1472 = ORIENTED_EDGE ( 'NONE', *, *, #18070, .T. ) ;
#1473 = DIRECTION ( 'NONE',  ( 0.000000000000000000, -1.000000000000000000, 0.000000000000000000 ) ) ;
#1474 = CARTESIAN_POINT ( 'NONE',  ( 11.08076314313121991, 13.15907583843444684, 5.707371360959808015 ) ) ;
#1475 = LINE ( 'NONE', #8221, #9766 ) ;
#1476 = PLANE ( 'NONE',  #5340 ) ;
#1477 = CARTESIAN_POINT ( 'NONE',  ( 12.76988556689188137, 18.82436523581427323, 5.780649009981873476 ) ) ;
#1478 = DIRECTION ( 'NONE',  ( -0.9964481331860212121, 0.000000000000000000, 0.08420877549337300871 ) ) ;
#1479 = CARTESIAN_POINT ( 'NONE',  ( 20.06462325295336413, -2.740908352756980193, -14.15992765561396105 ) ) ;
#1480 = VERTEX_POINT ( 'NONE', #4310 ) ;
#1481 = CARTESIAN_POINT ( 'NONE',  ( 0.000000000000000000, 0.000000000000000000, 0.000000000000000000 ) ) ;
#1482 = CYLINDRICAL_SURFACE ( 'NONE', #18394, 0.7950199999999985057 ) ;
#1483 = AXIS2_PLACEMENT_3D ( 'NONE', #17356, #2200, #12384 ) ;
#1484 = CIRCLE ( 'NONE', #3603, 1.983740000000000503 ) ;
#1485 = ORIENTED_EDGE ( 'NONE', *, *, #2953, .T. ) ;
#1486 = DIRECTION ( 'NONE',  ( -0.9579671649362032637, 0.000000000000000000, 0.2868778675745010664 ) ) ;
#1487 = EDGE_CURVE ( 'NONE', #20325, #10491, #6279, .T. ) ;
#1488 = CIRCLE ( 'NONE', #9595, 30.16249999999999076 ) ;
#1489 = CARTESIAN_POINT ( 'NONE',  ( 20.36422011069876348, -6.543713029916194301, -15.61347904700674860 ) ) ;
#1490 = ORIENTED_EDGE ( 'NONE', *, *, #10715, .F. ) ;
#1491 = STYLED_ITEM ( 'NONE', ( #1555 ), #20809 ) ;
#1492 = CARTESIAN_POINT ( 'NONE',  ( 5.544963268879691043, 15.56575848494070868, -1.416610689648610810 ) ) ;
#1493 = CARTESIAN_POINT ( 'NONE',  ( 3.121107721641948274, 20.34465986264832793, 2.720177380617953222 ) ) ;
#1494 = CARTESIAN_POINT ( 'NONE',  ( 28.87608719841374949, 29.75832250000000201, -15.73691681567849976 ) ) ;
#1495 = CARTESIAN_POINT ( 'NONE',  ( 8.143579141861840398, 10.68807868122940263, 1.737412375843639056 ) ) ;
#1496 = VECTOR ( 'NONE', #10087, 1000.000000000000114 ) ;
#1497 = CARTESIAN_POINT ( 'NONE',  ( 17.12726144548341267, -7.073893271879835964, -15.84366279292657609 ) ) ;
#1498 = FACE_OUTER_BOUND ( 'NONE', #6214, .T. ) ;
#1499 = VERTEX_POINT ( 'NONE', #1305 ) ;
#1500 = CARTESIAN_POINT ( 'NONE',  ( 8.362500416128090919, 20.24457714144503129, -0.2252561178185202018 ) ) ;
#1501 = CARTESIAN_POINT ( 'NONE',  ( 12.04632062715783825, 21.69057506433588145, 3.955334450274141211 ) ) ;
#1502 = CARTESIAN_POINT ( 'NONE',  ( 65.64431122251959039, 0.000000000000000000, -11.29787305743958115 ) ) ;
#1503 = EDGE_LOOP ( 'NONE', ( #2825, #2613, #15196, #20000 ) ) ;
#1504 = ORIENTED_EDGE ( 'NONE', *, *, #10980, .T. ) ;
#1505 = AXIS2_PLACEMENT_3D ( 'NONE', #9439, #21375, #6231 ) ;
#1506 = DIRECTION ( 'NONE',  ( 0.2490110332224850509, 0.000000000000000000, -0.9685006480810792739 ) ) ;
#1508 = CARTESIAN_POINT ( 'NONE',  ( 52.65345379380355695, 37.69740999999999786, -16.29354262597941982 ) ) ;
#1507 = CARTESIAN_POINT ( 'NONE',  ( 3.452510760150116376, 13.11091270743887982, 8.248611567737054173 ) ) ;
#1509 = VERTEX_POINT ( 'NONE', #21425 ) ;
#1510 = CARTESIAN_POINT ( 'NONE',  ( 7.499653097299838755, 16.51387688058736813, 8.389459965282956233 ) ) ;
#1511 = ORIENTED_EDGE ( 'NONE', *, *, #4111, .T. ) ;
#1512 = VERTEX_POINT ( 'NONE', #13051 ) ;
#1513 = AXIS2_PLACEMENT_3D ( 'NONE', #12024, #14937, #10368 ) ;
#1514 = EDGE_CURVE ( 'NONE', #18977, #107, #1416, .T. ) ;
#1515 = DIRECTION ( 'NONE',  ( 0.000000000000000000, 1.000000000000000000, 0.000000000000000000 ) ) ;
#1516 = EDGE_LOOP ( 'NONE', ( #5996, #3693 ) ) ;
#1517 = ADVANCED_FACE ( 'NONE', ( #19873 ), #19758, .T. ) ;
#1518 = CARTESIAN_POINT ( 'NONE',  ( 2.167641574481099731, 12.74517228915138212, 1.985490079943990516 ) ) ;
#1519 = CARTESIAN_POINT ( 'NONE',  ( 10.28844099665304412, 20.83333359141052199, -1.718030307083335595 ) ) ;
#1520 = AXIS2_PLACEMENT_3D ( 'NONE', #3677, #8317, #4998 ) ;
#1521 = PLANE ( 'NONE',  #18095 ) ;
#1522 = CARTESIAN_POINT ( 'NONE',  ( 54.11611804786240043, 1.984375000000000000, -30.58983753981140197 ) ) ;
#1523 = DIRECTION ( 'NONE',  ( 0.000000000000000000, 0.000000000000000000, -1.000000000000000000 ) ) ;
#1524 = CARTESIAN_POINT ( 'NONE',  ( 2.096007501654802319, 11.92778348172325309, 1.811772831717551213 ) ) ;
#1525 = VERTEX_POINT ( 'NONE', #18125 ) ;
#1526 = FACE_OUTER_BOUND ( 'NONE', #18731, .T. ) ;
#1527 = DIRECTION ( 'NONE',  ( 0.8667647648559581031, 0.000000000000000000, 0.4987171968201974948 ) ) ;
#1528 = DIRECTION ( 'NONE',  ( 0.000000000000000000, 1.000000000000000000, 0.000000000000000000 ) ) ;
#1529 = CARTESIAN_POINT ( 'NONE',  ( 53.57721252000833800, 37.93694508125481235, -16.14030231556136741 ) ) ;
#1530 = VECTOR ( 'NONE', #12478, 1000.000000000000114 ) ;
#1531 = ORIENTED_EDGE ( 'NONE', *, *, #360, .T. ) ;
#1532 = ORIENTED_EDGE ( 'NONE', *, *, #17236, .T. ) ;
#1533 = CARTESIAN_POINT ( 'NONE',  ( 12.92240294059410211, 14.85126536588636981, 6.483913497415390914 ) ) ;
#1534 = DIRECTION ( 'NONE',  ( 1.000000000000000000, 0.000000000000000000, 0.000000000000000000 ) ) ;
#1535 = VERTEX_POINT ( 'NONE', #11049 ) ;
#1536 = ADVANCED_FACE ( 'NONE', ( #12712 ), #21206, .F. ) ;
#1537 = ADVANCED_FACE ( 'NONE', ( #4632 ), #2983, .T. ) ;
#1538 = ORIENTED_EDGE ( 'NONE', *, *, #8761, .F. ) ;
#1539 = CARTESIAN_POINT ( 'NONE',  ( -12.30312499999999964, 30.56064500000000095, 8.731249999999999289 ) ) ;
#1540 = AXIS2_PLACEMENT_3D ( 'NONE', #3782, #466, #5769 ) ;
#1541 = ORIENTED_EDGE ( 'NONE', *, *, #4537, .F. ) ;
#1542 = CARTESIAN_POINT ( 'NONE',  ( 8.651812068854638937, 11.71838207857883241, 3.844930327028207806 ) ) ;
#1543 = EDGE_CURVE ( 'NONE', #10050, #7714, #3297, .T. ) ;
#1544 = AXIS2_PLACEMENT_3D ( 'NONE', #5510, #321, #15717 ) ;
#1545 = ADVANCED_FACE ( 'NONE', ( #14488, #9707 ), #1090, .F. ) ;
#1546 = DIRECTION ( 'NONE',  ( -0.6702301885068638887, 0.000000000000000000, -0.7421532822901570903 ) ) ;
#1547 = PLANE ( 'NONE',  #20270 ) ;
#1548 = CARTESIAN_POINT ( 'NONE',  ( 0.2490388986165102403, 18.99610975872131391, 0.7649840613554721447 ) ) ;
#1549 = DIRECTION ( 'NONE',  ( 0.9129422336036127072, 0.000000000000000000, -0.4080888115384278536 ) ) ;
#1550 = ORIENTED_EDGE ( 'NONE', *, *, #5921, .F. ) ;
#1551 = CARTESIAN_POINT ( 'NONE',  ( 3.152307289661677725, 19.27890597942106155, 7.411273792436298358 ) ) ;
#1552 = AXIS2_PLACEMENT_3D ( 'NONE', #9619, #13292, #21231 ) ;
#1553 = PLANE ( 'NONE',  #6412 ) ;
#1554 = CARTESIAN_POINT ( 'NONE',  ( 47.80475250345301674, -6.356984999999999886, -11.91473563638243327 ) ) ;
#1555 = PRESENTATION_STYLE_ASSIGNMENT (( #13509 ) ) ;
#1556 = ORIENTED_EDGE ( 'NONE', *, *, #5973, .T. ) ;
#1557 = CARTESIAN_POINT ( 'NONE',  ( 9.883904741205039812, 20.90551644660764197, -1.655877603440282675 ) ) ;
#1558 = LINE ( 'NONE', #4877, #10288 ) ;
#1559 = CARTESIAN_POINT ( 'NONE',  ( 9.165814705648051230, 13.36932551753513820, -2.800491248554054291 ) ) ;
#1560 = EDGE_LOOP ( 'NONE', ( #19520, #15225, #14345, #9159, #6722, #1134 ) ) ;
#1561 = EDGE_CURVE ( 'NONE', #16780, #6164, #2753, .T. ) ;
#1562 = AXIS2_PLACEMENT_3D ( 'NONE', #2373, #4142, #10880 ) ;
#1563 = EDGE_CURVE ( 'NONE', #1054, #8841, #14380, .T. ) ;
#1564 = EDGE_CURVE ( 'NONE', #21044, #4458, #13163, .T. ) ;
#1565 = CARTESIAN_POINT ( 'NONE',  ( 7.531365603956712285, 21.70037184525196139, 3.190346535578575615 ) ) ;
#1566 = FACE_OUTER_BOUND ( 'NONE', #20603, .T. ) ;
#1567 = CARTESIAN_POINT ( 'NONE',  ( 41.78116128337411794, 34.52875999999999834, 7.392073290253172502 ) ) ;
#1568 = CARTESIAN_POINT ( 'NONE',  ( 6.939857573655906720, 18.57054895600834143, 7.059575150324737258 ) ) ;
#1569 = CARTESIAN_POINT ( 'NONE',  ( -15.39353573898878658, 34.79968030885680008, -10.30107656633069979 ) ) ;
#1570 = AXIS2_PLACEMENT_3D ( 'NONE', #3806, #14001, #17411 ) ;
#1571 = ORIENTED_EDGE ( 'NONE', *, *, #1634, .T. ) ;
#1572 = DIRECTION ( 'NONE',  ( -0.7776383362760926898, 0.000000000000000000, 0.6287118719681938916 ) ) ;
#1573 = CARTESIAN_POINT ( 'NONE',  ( 11.73484804242726298, 13.86399106732309328, 6.608254899136346339 ) ) ;
#1574 = AXIS2_PLACEMENT_3D ( 'NONE', #19977, #2980, #16575 ) ;
#1575 = CARTESIAN_POINT ( 'NONE',  ( -0.2353009082112856032, 21.11857065418899992, 4.744919637712884608 ) ) ;
#1576 = DIRECTION ( 'NONE',  ( 0.000000000000000000, 1.000000000000000000, 0.000000000000000000 ) ) ;
#1577 = CARTESIAN_POINT ( 'NONE',  ( 41.71184157647478230, 38.88803500000000213, -2.134205101306931862 ) ) ;
#1578 = CARTESIAN_POINT ( 'NONE',  ( 2.479339246688891052, 12.01113885212942201, 3.583524443125778891 ) ) ;
#1579 = LINE ( 'NONE', #11435, #21377 ) ;
#1580 = CARTESIAN_POINT ( 'NONE',  ( 14.40215569916422922, -8.180188028388664989, -16.42876195537290585 ) ) ;
#1581 = DIRECTION ( 'NONE',  ( -0.9685006480810793850, 0.000000000000000000, -0.2490110332224846623 ) ) ;
#1582 = VERTEX_POINT ( 'NONE', #19437 ) ;
#1583 = DIRECTION ( 'NONE',  ( 0.2868778675745011220, 0.000000000000000000, 0.9579671649362034858 ) ) ;
#1584 = CARTESIAN_POINT ( 'NONE',  ( 10.98060958781924690, 12.63125357519729164, 5.207718750913196359 ) ) ;
#1585 = PLANE ( 'NONE',  #593 ) ;
#1586 = ORIENTED_EDGE ( 'NONE', *, *, #5324, .F. ) ;
#1587 = EDGE_CURVE ( 'NONE', #5833, #21613, #9486, .T. ) ;
#1588 = CARTESIAN_POINT ( 'NONE',  ( 12.92686589858350565, 12.55799597913518184, 4.809958993587978959 ) ) ;
#1589 = CARTESIAN_POINT ( 'NONE',  ( 26.59062499999999929, 2.380615000000000148, 8.335010000000000474 ) ) ;
#1590 = CARTESIAN_POINT ( 'NONE',  ( 6.380166963026771221, 10.92343582149830183, 2.794643371853744007 ) ) ;
#1591 = CARTESIAN_POINT ( 'NONE',  ( 10.89278871826026496, -3.741510472769750351, -15.20017649982984409 ) ) ;
#1593 = CARTESIAN_POINT ( 'NONE',  ( -29.36874999999999858, 30.16440499999999858, 8.731249999999999289 ) ) ;
#1592 = CARTESIAN_POINT ( 'NONE',  ( 1.550976474600018085, 20.56989294761467946, 5.021185002739427361 ) ) ;
#1594 = EDGE_LOOP ( 'NONE', ( #10062, #8009, #14700, #9478, #16584, #21246 ) ) ;
#1595 = CARTESIAN_POINT ( 'NONE',  ( 19.84534036711146143, -1.573540299197002224, -15.46898262837090243 ) ) ;
#1596 = EDGE_LOOP ( 'NONE', ( #17698, #10706, #3633, #1414 ) ) ;
#1597 = CARTESIAN_POINT ( 'NONE',  ( 6.112021107885185600, 11.58565454437474251, 2.923295850109377536 ) ) ;
#1598 = ORIENTED_EDGE ( 'NONE', *, *, #13900, .F. ) ;
#1599 = CARTESIAN_POINT ( 'NONE',  ( 11.90896688976436302, 20.94853845629116051, 3.658657855874824172 ) ) ;
#1600 = CARTESIAN_POINT ( 'NONE',  ( 12.90481261863918938, 18.46417960692862437, 6.065349631274771447 ) ) ;
#1601 = DIRECTION ( 'NONE',  ( -0.9685006480810791629, 0.000000000000000000, -0.2490110332224850231 ) ) ;
#1602 = CARTESIAN_POINT ( 'NONE',  ( 8.186312780807948997, 21.32987559984598391, 5.068732912542537328 ) ) ;
#1603 = AXIS2_PLACEMENT_3D ( 'NONE', #8646, #3680, #10425 ) ;
#1604 = CARTESIAN_POINT ( 'NONE',  ( 14.65560158155272674, -7.011384195667019981, -16.35874738822244723 ) ) ;
#1605 = CYLINDRICAL_SURFACE ( 'NONE', #14505, 30.16250000000000497 ) ;
#1606 = ORIENTED_EDGE ( 'NONE', *, *, #68, .T. ) ;
#1607 = CARTESIAN_POINT ( 'NONE',  ( 9.675305929993816889, 20.98082586346679435, 3.267053697050358085 ) ) ;
#1608 = CARTESIAN_POINT ( 'NONE',  ( 10.98487345271878901, 19.57756785145604184, 6.723427973997481821 ) ) ;
#1609 = B_SPLINE_CURVE_WITH_KNOTS ( 'NONE', 3,
 ( #21823, #20148, #3475, #10325, #18716, #15209, #18393, #11777, #17073, #10211, #10106, #20257, #15434, #1805, #260, #10003, #18609, #16854, #1695, #16757, #4913, #20472, #5023, #6577, #12104, #20041, #18505, #7002, #16955, #11660, #6677, #1597, #13770, #8552, #5339, #20362, #18830, #15108, #8434, #15328, #3699, #10441, #152 ),
 .UNSPECIFIED., .F., .F.,
 ( 4, 3, 3, 3, 3, 3, 3, 3, 3, 3, 3, 3, 3, 3, 4 ),
 ( 0.000000000000000000, 0.09090909086959420016, 0.1818181817392079958, 0.2500562842553700205, 0.2727272726088130206, 0.3636363634784169907, 0.4545454543480210163, 0.5000905312070750286, 0.5454545452175250109, 0.6363636360871299802, 0.7272727269567340613, 0.7500720420152089396, 0.8181818178263380315, 0.9090909086959420016, 0.9999999995655460827 ),
 .UNSPECIFIED. ) ;
#1610 = CARTESIAN_POINT ( 'NONE',  ( 53.95242430215955665, 38.88803500000000213, -23.51676380836238067 ) ) ;
#1611 = ORIENTED_EDGE ( 'NONE', *, *, #18172, .F. ) ;
#1612 = ORIENTED_EDGE ( 'NONE', *, *, #3894, .T. ) ;
#1613 = ADVANCED_FACE ( 'NONE', ( #17904 ), #3086, .F. ) ;
#1614 = DIRECTION ( 'NONE',  ( 0.000000000000000000, 1.000000000000000000, 0.000000000000000000 ) ) ;
#1616 = PLANE ( 'NONE',  #9906 ) ;
#1615 = CARTESIAN_POINT ( 'NONE',  ( 3.704058153803886366, 12.19654146317258103, 0.4088179348593441453 ) ) ;
#1617 = VERTEX_POINT ( 'NONE', #7833 ) ;
#1618 = CARTESIAN_POINT ( 'NONE',  ( 7.229408460074554732, 18.55040875409351031, 7.925878126512573729 ) ) ;
#1619 = VERTEX_POINT ( 'NONE', #14609 ) ;
#1620 = ORIENTED_EDGE ( 'NONE', *, *, #12085, .F. ) ;
#1621 = CARTESIAN_POINT ( 'NONE',  ( 38.23013820809905638, 34.52875999999999834, -14.22485453658974031 ) ) ;
#1622 = VERTEX_POINT ( 'NONE', #21317 ) ;
#1623 = CARTESIAN_POINT ( 'NONE',  ( 49.72033008250774344, 42.06303499999999929, -2.687827786179598277 ) ) ;
#1624 = DIRECTION ( 'NONE',  ( 0.000000000000000000, 1.000000000000000000, 0.000000000000000000 ) ) ;
#1625 = CARTESIAN_POINT ( 'NONE',  ( 2.065058272705286413, 12.01021496580790782, 1.672441337454303900 ) ) ;
#1626 = EDGE_LOOP ( 'NONE', ( #16316, #15503, #7681, #7730 ) ) ;
#1627 = DIRECTION ( 'NONE',  ( 0.5222415575336524229, 0.000000000000000000, 0.8527976052879281399 ) ) ;
#1628 = DIRECTION ( 'NONE',  ( 0.9579671649362032637, 0.000000000000000000, -0.2868778675745012885 ) ) ;
#1629 = CARTESIAN_POINT ( 'NONE',  ( 46.03750000000000142, 1.984375000000000000, -10.31874999999999964 ) ) ;
#1630 = LINE ( 'NONE', #8478, #12784 ) ;
#1631 = PLANE ( 'NONE',  #5961 ) ;
#1632 = VERTEX_POINT ( 'NONE', #6178 ) ;
#1633 = ORIENTED_EDGE ( 'NONE', *, *, #15870, .F. ) ;
#1634 = EDGE_CURVE ( 'NONE', #1329, #15472, #9617, .T. ) ;
#1635 = CARTESIAN_POINT ( 'NONE',  ( 11.00015320311062439, 17.51254433608867700, 6.806021621348003592 ) ) ;
#1636 = DIRECTION ( 'NONE',  ( 0.000000000000000000, 1.000000000000000000, 0.000000000000000000 ) ) ;
#1637 = ORIENTED_EDGE ( 'NONE', *, *, #6499, .T. ) ;
#1638 = ORIENTED_EDGE ( 'NONE', *, *, #8866, .F. ) ;
#1639 = LINE ( 'NONE', #3320, #14876 ) ;
#1640 = AXIS2_PLACEMENT_3D ( 'NONE', #18596, #3466, #10200 ) ;
#1641 = ORIENTED_EDGE ( 'NONE', *, *, #12188, .F. ) ;
#1642 = CARTESIAN_POINT ( 'NONE',  ( 8.545873062880019688, 11.61005284472577159, 3.376861938372578198 ) ) ;
#1643 = CARTESIAN_POINT ( 'NONE',  ( 3.430718016658220293, 15.33128678211075702, 8.333009793459709158 ) ) ;
#1644 = EDGE_CURVE ( 'NONE', #11015, #3875, #17773, .T. ) ;
#1645 = CARTESIAN_POINT ( 'NONE',  ( -7.949728765564807453, 33.79463943364264367, -34.47798802950575237 ) ) ;
#1646 = DIRECTION ( 'NONE',  ( 0.000000000000000000, -1.000000000000000000, 0.000000000000000000 ) ) ;
#1647 = CARTESIAN_POINT ( 'NONE',  ( -0.1672139265598213131, 16.21125157041092635, 0.03678197978728087181 ) ) ;
#1648 = CARTESIAN_POINT ( 'NONE',  ( -4.157227781567939928, 9.129395000000000593, 0.1758860224507720060 ) ) ;
#1649 = CIRCLE ( 'NONE', #18962, 3.970020000000001215 ) ;
#1650 = EDGE_LOOP ( 'NONE', ( #3417, #10618, #16697, #7905 ) ) ;
#1651 = CARTESIAN_POINT ( 'NONE',  ( 1.377977696595360291, 12.31440956997844083, 6.220707012221055265 ) ) ;
#1652 = FACE_OUTER_BOUND ( 'NONE', #18846, .T. ) ;
#1653 = CARTESIAN_POINT ( 'NONE',  ( 52.89438837027574181, -7.516544198863053694, -16.93158128026265885 ) ) ;
#1654 = FILL_AREA_STYLE ('',( #4874 ) ) ;
#1655 = CARTESIAN_POINT ( 'NONE',  ( -17.46249999999999858, 30.56064500000000095, 0.000000000000000000 ) ) ;
#1656 = VERTEX_POINT ( 'NONE', #191 ) ;
#1657 = EDGE_CURVE ( 'NONE', #8399, #20861, #20397, .T. ) ;
#1658 = CARTESIAN_POINT ( 'NONE',  ( 7.867384389574832326, 10.77439257666578243, 1.834364527281745483 ) ) ;
#1659 = ADVANCED_FACE ( 'NONE', ( #17113 ), #3627, .F. ) ;
#1660 = DIRECTION ( 'NONE',  ( 0.08420877549337300871, 0.000000000000000000, 0.9964481331860212121 ) ) ;
#1661 = CARTESIAN_POINT ( 'NONE',  ( 11.68885165013066185, 21.89103689682439224, 3.044870294398752453 ) ) ;
#1662 = ORIENTED_EDGE ( 'NONE', *, *, #3097, .T. ) ;
#1663 = CARTESIAN_POINT ( 'NONE',  ( 8.590151053309458717, 10.83020630611641266, 3.529432304467389425 ) ) ;
#1664 = CARTESIAN_POINT ( 'NONE',  ( 3.480677399789653848, 14.96908372069038684, 8.311097829955567562 ) ) ;
#1665 = DIRECTION ( 'NONE',  ( -0.5087559856598092844, 0.000000000000000000, -0.8609107660235849613 ) ) ;
#1666 = DIRECTION ( 'NONE',  ( -0.2868778675745011220, 0.000000000000000000, -0.9579671649362034858 ) ) ;
#1667 = AXIS2_PLACEMENT_3D ( 'NONE', #11026, #9465, #4401 ) ;
#1668 = CARTESIAN_POINT ( 'NONE',  ( 54.29867169743560140, 0.000000000000000000, -30.73743011777780154 ) ) ;
#1669 = CARTESIAN_POINT ( 'NONE',  ( 8.600866579439452764, 11.08822532131044092, 1.666493167020851818 ) ) ;
#1670 = EDGE_CURVE ( 'NONE', #1656, #13806, #15669, .T. ) ;
#1671 = CARTESIAN_POINT ( 'NONE',  ( 2.903384396171142967, 20.92902966678202148, 1.811677702956517866 ) ) ;
#1672 = CARTESIAN_POINT ( 'NONE',  ( 28.97711086133420366, 32.54502000000000095, -10.71499000000000024 ) ) ;
#1673 = CARTESIAN_POINT ( 'NONE',  ( 20.18250336069275974, -0.9908562680277209767, -14.77328602232822519 ) ) ;
#1674 = CARTESIAN_POINT ( 'NONE',  ( -0.01591978660616180652, 15.70515029433102860, 0.7746393958769953736 ) ) ;
#1675 = DIRECTION ( 'NONE',  ( 0.000000000000000000, 1.000000000000000000, 0.000000000000000000 ) ) ;
#1676 = DIRECTION ( 'NONE',  ( 0.9685006480810793850, 0.000000000000000000, 0.2490110332224846623 ) ) ;
#1677 = CARTESIAN_POINT ( 'NONE',  ( 10.97108191230651109, -4.649804219968682872, -17.12215967864936772 ) ) ;
#1678 = LINE ( 'NONE', #15312, #7096 ) ;
#1679 = VECTOR ( 'NONE', #5420, 1000.000000000000000 ) ;
#1680 = ORIENTED_EDGE ( 'NONE', *, *, #21692, .T. ) ;
#1681 = EDGE_CURVE ( 'NONE', #14418, #11144, #11913, .T. ) ;
#1682 = CARTESIAN_POINT ( 'NONE',  ( 10.20773825118543421, 21.26060903501195298, 4.752181056839726025 ) ) ;
#1683 = DIRECTION ( 'NONE',  ( 0.000000000000000000, 1.000000000000000000, 0.000000000000000000 ) ) ;
#1684 = DIRECTION ( 'NONE',  ( 1.000000000000000000, 0.000000000000000000, 0.000000000000000000 ) ) ;
#1685 = CARTESIAN_POINT ( 'NONE',  ( 12.74520702676420392, 11.91691794096125534, 3.970093380836815289 ) ) ;
#1686 = CARTESIAN_POINT ( 'NONE',  ( 5.447351731530780228, 30.56064500000000095, 0.8930339070797439494 ) ) ;
#1687 = CARTESIAN_POINT ( 'NONE',  ( 19.35144069079204954, -5.834156456616997666, -15.24901388582027195 ) ) ;
#1689 = CARTESIAN_POINT ( 'NONE',  ( 20.53156612299923012, -1.359449706705494254, -15.90722162142133733 ) ) ;
#1688 = CARTESIAN_POINT ( 'NONE',  ( 6.007628987977455814, 11.57021355890683978, 2.543656572248523595 ) ) ;
#1690 = ORIENTED_EDGE ( 'NONE', *, *, #5153, .F. ) ;
#1691 = CARTESIAN_POINT ( 'NONE',  ( 0.000000000000000000, 0.000000000000000000, 0.000000000000000000 ) ) ;
#1692 = LINE ( 'NONE', #3473, #20854 ) ;
#1693 = CARTESIAN_POINT ( 'NONE',  ( 3.738535879684092400, 15.59511426254074173, -0.5956637481122312172 ) ) ;
#1694 = CARTESIAN_POINT ( 'NONE',  ( 46.03750000000000142, 0.000000000000000000, -10.31874999999999964 ) ) ;
#1695 = CARTESIAN_POINT ( 'NONE',  ( 6.010820999879410209, 11.26290339936039153, 2.930039796312023270 ) ) ;
#1696 = AXIS2_PLACEMENT_3D ( 'NONE', #16112, #944, #14450 ) ;
#1697 = CARTESIAN_POINT ( 'NONE',  ( 11.48491928014121122, -6.408048376592000217, -17.19675141021907550 ) ) ;
#1698 = VERTEX_POINT ( 'NONE', #16886 ) ;
#1699 = CARTESIAN_POINT ( 'NONE',  ( 5.792450260185113109, 12.69966494906990206, 0.1988901986138334466 ) ) ;
#1700 = CARTESIAN_POINT ( 'NONE',  ( 4.007488201923330884, 20.44159178862518189, 5.038468532300615088 ) ) ;
#1701 = EDGE_CURVE ( 'NONE', #13851, #8918, #7179, .T. ) ;
#1702 = CARTESIAN_POINT ( 'NONE',  ( 8.546142373387299429, 20.63131727706956298, 0.1902865990017700848 ) ) ;
#1703 = CARTESIAN_POINT ( 'NONE',  ( 2.000976789916291132, 15.60105019847626551, 9.484685655146686045 ) ) ;
#1704 = EDGE_CURVE ( 'NONE', #17862, #13475, #2935, .T. ) ;
#1705 = CARTESIAN_POINT ( 'NONE',  ( 11.53313857698689837, 20.24893436370382105, -3.119838056082069766 ) ) ;
#1706 = PRODUCT_DEFINITION_FORMATION_WITH_SPECIFIED_SOURCE ( 'ANY', '', #14278, .NOT_KNOWN. ) ;
#1707 = CARTESIAN_POINT ( 'NONE',  ( 12.66650400994676140, -5.505089894041057974, -16.74975958372730389 ) ) ;
#1708 = FACE_OUTER_BOUND ( 'NONE', #17654, .T. ) ;
#1709 = ORIENTED_EDGE ( 'NONE', *, *, #4496, .T. ) ;
#1710 = CARTESIAN_POINT ( 'NONE',  ( 9.829229519957147332, 20.86878119585347235, 3.677952529984052532 ) ) ;
#1711 = CARTESIAN_POINT ( 'NONE',  ( 9.396859391623667790, 12.85930032217342145, 6.944093101771448673 ) ) ;
#1712 = CARTESIAN_POINT ( 'NONE',  ( -15.41509608936259035, -4.609114529603660415, -10.31276839742836415 ) ) ;
#1713 = B_SPLINE_CURVE_WITH_KNOTS ( 'NONE', 3,
 ( #12498, #7513, #19221, #4190, #10495, #15718, #17682, #2534 ),
 .UNSPECIFIED., .F., .F.,
 ( 4, 2, 2, 4 ),
 ( 0.000000000000000000, 0.2499999999999987232, 0.4999999999999974465, 1.000000000000000000 ),
 .UNSPECIFIED. ) ;
#1714 = VERTEX_POINT ( 'NONE', #6609 ) ;
#1715 = VERTEX_POINT ( 'NONE', #6720 ) ;
#1716 = AXIS2_PLACEMENT_3D ( 'NONE', #4854, #11488, #15146 ) ;
#1717 = CARTESIAN_POINT ( 'NONE',  ( 11.24737647850577993, 19.43957250000000059, -3.746985211334052046 ) ) ;
#1718 = CARTESIAN_POINT ( 'NONE',  ( 10.98588874387031211, 13.67752812875329838, -3.721421232128317769 ) ) ;
#1720 = CYLINDRICAL_SURFACE ( 'NONE', #9198, 5.357812499999999645 ) ;
#1719 = CARTESIAN_POINT ( 'NONE',  ( 5.043785943435923791, 12.41500460647656112, 7.215820400045201310 ) ) ;
#1721 = VERTEX_POINT ( 'NONE', #6934 ) ;
#1722 = CARTESIAN_POINT ( 'NONE',  ( 5.768991567460251879, 21.49153886321743201, 4.134389838676610474 ) ) ;
#1723 = DIRECTION ( 'NONE',  ( 0.000000000000000000, 1.000000000000000000, 0.000000000000000000 ) ) ;
#1724 = ORIENTED_EDGE ( 'NONE', *, *, #15650, .T. ) ;
#1725 = DIRECTION ( 'NONE',  ( 0.9959941601142464629, 0.000000000000000000, 0.08941830359784661009 ) ) ;
#1726 = ORIENTED_EDGE ( 'NONE', *, *, #19630, .T. ) ;
#1727 = EDGE_CURVE ( 'NONE', #6920, #17175, #14614, .T. ) ;
#1728 = AXIS2_PLACEMENT_3D ( 'NONE', #5068, #1959, #20517 ) ;
#1729 = CYLINDRICAL_SURFACE ( 'NONE', #21257, 0.5080000000000014504 ) ;
#1730 = CARTESIAN_POINT ( 'NONE',  ( -14.90829243662735060, -2.075094819660129986, -10.03143607188699526 ) ) ;
#1731 = PRODUCT_DEFINITION_SHAPE ( 'NONE', 'NONE',  #21886 ) ;
#1732 = FACE_OUTER_BOUND ( 'NONE', #14774, .T. ) ;
#1733 = CARTESIAN_POINT ( 'NONE',  ( 2.827832784706104441, 20.82732273834332304, 1.888333759270794499 ) ) ;
#1734 = VECTOR ( 'NONE', #18310, 1000.000000000000114 ) ;
#1735 = VERTEX_POINT ( 'NONE', #20293 ) ;
#1736 = DIRECTION ( 'NONE',  ( 0.000000000000000000, 1.000000000000000000, 0.000000000000000000 ) ) ;
#1737 = CARTESIAN_POINT ( 'NONE',  ( 46.03750000000000142, 32.54502000000000095, -10.31874999999999964 ) ) ;
#1738 = CARTESIAN_POINT ( 'NONE',  ( 9.321907506464571114, 3.084972983906390631, -16.32229253314513784 ) ) ;
#1739 = LINE ( 'NONE', #5067, #13841 ) ;
#1741 = CARTESIAN_POINT ( 'NONE',  ( 17.15398648756978517, -6.962794673133186230, -14.62314114746725302 ) ) ;
#1740 = CARTESIAN_POINT ( 'NONE',  ( 24.26606285357373594, 29.75832250000000201, -16.92219937337620195 ) ) ;
#1742 = ORIENTED_EDGE ( 'NONE', *, *, #19248, .F. ) ;
#1743 = EDGE_LOOP ( 'NONE', ( #7465, #6376, #15613, #2042 ) ) ;
#1744 = CARTESIAN_POINT ( 'NONE',  ( 7.472981172757774182, 13.15088303497838140, -1.026857982812649395 ) ) ;
#1745 = CARTESIAN_POINT ( 'NONE',  ( 3.287836056772957427, 11.90013693509636106, 6.878074374375073852 ) ) ;
#1746 = ORIENTED_EDGE ( 'NONE', *, *, #14225, .F. ) ;
#1747 = ORIENTED_EDGE ( 'NONE', *, *, #6828, .T. ) ;
#1748 = DIRECTION ( 'NONE',  ( 0.000000000000000000, 1.000000000000000000, 0.000000000000000000 ) ) ;
#1749 = ORIENTED_EDGE ( 'NONE', *, *, #20617, .T. ) ;
#1750 = CARTESIAN_POINT ( 'NONE',  ( 9.154392979045368861, 13.35535808052676110, 6.215094776725202053 ) ) ;
#1751 = EDGE_CURVE ( 'NONE', #4180, #17367, #17419, .T. ) ;
#1752 = DIRECTION ( 'NONE',  ( 0.9999603561554373243, 0.000000000000000000, -0.008904275236710241376 ) ) ;
#1753 = CARTESIAN_POINT ( 'NONE',  ( 29.37324403177899868, 0.000000000000000000, -10.70578951775076071 ) ) ;
#1754 = DIRECTION ( 'NONE',  ( 0.000000000000000000, 1.000000000000000000, 0.000000000000000000 ) ) ;
#1755 = CARTESIAN_POINT ( 'NONE',  ( 0.3034835435385529467, 19.20128088117248311, 0.8914707698310011530 ) ) ;
#1756 = FACE_OUTER_BOUND ( 'NONE', #854, .T. ) ;
#1757 = ORIENTED_EDGE ( 'NONE', *, *, #17479, .F. ) ;
#1758 = CARTESIAN_POINT ( 'NONE',  ( 5.344873306944882607, 17.31775664876643006, 7.991828959977699043 ) ) ;
#1759 = DIRECTION ( 'NONE',  ( -0.000000000000000000, -1.000000000000000000, 0.000000000000000000 ) ) ;
#1760 = DIRECTION ( 'NONE',  ( 0.9784543669157820256, 0.000000000000000000, 0.2064631973583577473 ) ) ;
#1761 = LINE ( 'NONE', #8507, #17257 ) ;
#1762 = VERTEX_POINT ( 'NONE', #20081 ) ;
#1763 = CARTESIAN_POINT ( 'NONE',  ( 8.327167164761551277, 10.82907781979698214, 3.764246136999646275 ) ) ;
#1764 = VECTOR ( 'NONE', #9628, 1000.000000000000000 ) ;
#1765 = CARTESIAN_POINT ( 'NONE',  ( 13.08108576808625045, 18.67096353113900520, 6.700927112183967971 ) ) ;
#1766 = ORIENTED_EDGE ( 'NONE', *, *, #20682, .F. ) ;
#1767 = CIRCLE ( 'NONE', #6716, 0.5080000000000000071 ) ;
#1768 = VERTEX_POINT ( 'NONE', #4947 ) ;
#1769 = CARTESIAN_POINT ( 'NONE',  ( 9.343037286256407725, 12.92999292743880702, 6.861527116923473280 ) ) ;
#1770 = CARTESIAN_POINT ( 'NONE',  ( 1.122858828880666460, 18.50002798056422293, 8.328379096489866740 ) ) ;
#1771 = DIRECTION ( 'NONE',  ( 0.000000000000000000, 1.000000000000000000, 0.000000000000000000 ) ) ;
#1772 = EDGE_CURVE ( 'NONE', #4527, #1656, #18757, .T. ) ;
#1773 = CARTESIAN_POINT ( 'NONE',  ( 39.58386072796550081, 38.88803500000000213, -4.490541772578183100 ) ) ;
#1774 = AXIS2_PLACEMENT_3D ( 'NONE', #10053, #8282, #6290 ) ;
#1775 = CARTESIAN_POINT ( 'NONE',  ( 1.852730722019251930, 20.39130814012998982, 4.938901323796075715 ) ) ;
#1776 = FACE_OUTER_BOUND ( 'NONE', #9027, .T. ) ;
#1777 = EDGE_CURVE ( 'NONE', #13169, #13930, #7878, .T. ) ;
#1778 = CARTESIAN_POINT ( 'NONE',  ( 9.570742583039159257, 15.35048014666334559, -3.380060443643036816 ) ) ;
#1779 = ADVANCED_FACE ( 'NONE', ( #1526 ), #8369, .F. ) ;
#1780 = AXIS2_PLACEMENT_3D ( 'NONE', #17428, #17535, #277 ) ;
#1781 = CARTESIAN_POINT ( 'NONE',  ( 3.570643486829286228, 15.44796252803982206, -1.483651343954088597 ) ) ;
#1782 = CARTESIAN_POINT ( 'NONE',  ( 0.2641497867371597752, 26.98019749999999917, -24.43980549416641068 ) ) ;
#1783 = CARTESIAN_POINT ( 'NONE',  ( 20.22951472560300346, -1.344520626714845069, -14.75553331646387711 ) ) ;
#1784 = CARTESIAN_POINT ( 'NONE',  ( 5.344534969970771598, 14.21717427261922673, 7.627733794437622450 ) ) ;
#1785 = B_SPLINE_CURVE_WITH_KNOTS ( 'NONE', 3,
 ( #10743, #10628, #670, #19132 ),
 .UNSPECIFIED., .F., .F.,
 ( 4, 4 ),
 ( 0.000000000000000000, 1.000000000000000000 ),
 .UNSPECIFIED. ) ;
#1786 = DIRECTION ( 'NONE',  ( 0.9685006480810794960, 0.000000000000000000, 0.2490110332224836354 ) ) ;
#1787 = FACE_OUTER_BOUND ( 'NONE', #13799, .T. ) ;
#1788 = CARTESIAN_POINT ( 'NONE',  ( 14.12322331492428873, -8.081744716033297138, -16.48945220907392795 ) ) ;
#1789 = DIRECTION ( 'NONE',  ( 0.000000000000000000, -1.000000000000000000, 0.000000000000000000 ) ) ;
#1790 = VECTOR ( 'NONE', #4709, 1000.000000000000000 ) ;
#1791 = ORIENTED_EDGE ( 'NONE', *, *, #11880, .T. ) ;
#1792 = CARTESIAN_POINT ( 'NONE',  ( 11.10692670746270316, 13.33981709075777644, 5.846286987766022847 ) ) ;
#1793 = AXIS2_PLACEMENT_3D ( 'NONE', #6813, #5365, #8679 ) ;
#1794 = CARTESIAN_POINT ( 'NONE',  ( 10.44282649712041433, 20.84799543583206116, 5.382918864209185195 ) ) ;
#1795 = LINE ( 'NONE', #17058, #10488 ) ;
#1796 = ORIENTED_EDGE ( 'NONE', *, *, #10074, .F. ) ;
#1797 = CARTESIAN_POINT ( 'NONE',  ( 13.07577240337103319, 13.46997794477539578, 5.567646671893168531 ) ) ;
#1798 = CARTESIAN_POINT ( 'NONE',  ( 71.04062499999999147, 0.000000000000000000, -10.31874999999999964 ) ) ;
#1800 = CARTESIAN_POINT ( 'NONE',  ( 3.805353748838121053, -14.84248999999999974, -22.18284873352824960 ) ) ;
#1799 = CARTESIAN_POINT ( 'NONE',  ( 1.650854728546951256, 13.47654819534602133, 1.014815903823355736 ) ) ;
#1801 = ORIENTED_EDGE ( 'NONE', *, *, #20190, .T. ) ;
#1802 = PRODUCT_CONTEXT ( 'NONE', #11877, 'mechanical' ) ;
#1803 = EDGE_CURVE ( 'NONE', #16972, #11670, #19980, .T. ) ;
#1804 = LINE ( 'NONE', #18606, #19796 ) ;
#1805 = CARTESIAN_POINT ( 'NONE',  ( 6.072633846711956274, 11.08857437794745060, 2.898804142493843106 ) ) ;
#1806 = VECTOR ( 'NONE', #9637, 1000.000000000000000 ) ;
#1807 = CIRCLE ( 'NONE', #18754, 0.5079999999999985638 ) ;
#1808 = AXIS2_PLACEMENT_3D ( 'NONE', #10508, #6965, #15505 ) ;
#1809 = ORIENTED_EDGE ( 'NONE', *, *, #492, .F. ) ;
#1810 = CARTESIAN_POINT ( 'NONE',  ( 7.518022070815600699, 21.00575954651474220, 3.199318596789233027 ) ) ;
#1811 = EDGE_CURVE ( 'NONE', #7476, #17693, #13183, .T. ) ;
#1812 = CARTESIAN_POINT ( 'NONE',  ( 9.745609355272696561, 21.05303134726939973, 3.406578442638684034 ) ) ;
#1813 = CARTESIAN_POINT ( 'NONE',  ( 5.930740481208400361, 15.68947463651248420, 8.349508172414736862 ) ) ;
#1814 = CARTESIAN_POINT ( 'NONE',  ( 6.883721427746540833, 11.28756208157694019, 5.058899341199012412 ) ) ;
#1815 = VECTOR ( 'NONE', #20879, 1000.000000000000000 ) ;
#1816 = EDGE_CURVE ( 'NONE', #6920, #19435, #12114, .T. ) ;
#1817 = CARTESIAN_POINT ( 'NONE',  ( 14.52745126260834141, -6.964383640051551083, -16.38517187279768095 ) ) ;
#1818 = CARTESIAN_POINT ( 'NONE',  ( 11.81489480681374715, -4.423560566030090513, -15.68132100509055782 ) ) ;
#1819 = VERTEX_POINT ( 'NONE', #20194 ) ;
#1820 = CARTESIAN_POINT ( 'NONE',  ( 10.62526409008942530, 19.44399953203486930, 5.732770084512769593 ) ) ;
#1821 = CARTESIAN_POINT ( 'NONE',  ( 8.188127480685322368, 10.68876677029517985, 1.724185228589610430 ) ) ;
#1822 = AXIS2_PLACEMENT_3D ( 'NONE', #12937, #19751, #16572 ) ;
#1823 = ORIENTED_EDGE ( 'NONE', *, *, #16213, .F. ) ;
#1824 = EDGE_LOOP ( 'NONE', ( #17987, #8783, #945, #11646 ) ) ;
#1825 = CIRCLE ( 'NONE', #3243, 1.984374999999998890 ) ;
#1826 = CIRCLE ( 'NONE', #21612, 9.524999999999996803 ) ;
#1827 = DIRECTION ( 'NONE',  ( 0.000000000000000000, -1.000000000000000000, 0.000000000000000000 ) ) ;
#1828 = CARTESIAN_POINT ( 'NONE',  ( 38.96848998618624904, -7.547609999999999708, -3.934807454472129429 ) ) ;
#1830 = DIRECTION ( 'NONE',  ( -0.9685006480810792739, 0.000000000000000000, -0.2490110332224846346 ) ) ;
#1829 = CARTESIAN_POINT ( 'NONE',  ( 4.288727190992245752, 11.05839472165502180, 3.905392380839078914 ) ) ;
#1831 = ORIENTED_EDGE ( 'NONE', *, *, #17908, .T. ) ;
#1832 = CARTESIAN_POINT ( 'NONE',  ( 7.411476586714386805, 17.43287269264193995, 8.287351011025366532 ) ) ;
#1833 = EDGE_CURVE ( 'NONE', #8981, #14185, #11815, .T. ) ;
#1834 = EDGE_CURVE ( 'NONE', #7504, #3737, #15369, .T. ) ;
#1835 = VECTOR ( 'NONE', #1851, 1000.000000000000114 ) ;
#1836 = CARTESIAN_POINT ( 'NONE',  ( 3.805353748838121053, 36.51313500000000545, -22.18284873352824960 ) ) ;
#1837 = EDGE_CURVE ( 'NONE', #16799, #19840, #20975, .T. ) ;
#1838 = ORIENTED_EDGE ( 'NONE', *, *, #10629, .F. ) ;
#1839 = DIRECTION ( 'NONE',  ( 0.000000000000000000, 1.000000000000000000, 0.000000000000000000 ) ) ;
#1840 = ORIENTED_EDGE ( 'NONE', *, *, #2050, .F. ) ;
#1841 = CARTESIAN_POINT ( 'NONE',  ( 1.904339175427839370, 14.42031344806993509, 0.5205678229890007280 ) ) ;
#1842 = VECTOR ( 'NONE', #10307, 1000.000000000000000 ) ;
#1843 = LINE ( 'NONE', #15037, #8191 ) ;
#1844 = CARTESIAN_POINT ( 'NONE',  ( -17.46249999999999858, 33.73373999999999739, 0.000000000000000000 ) ) ;
#1845 = CARTESIAN_POINT ( 'NONE',  ( 1.804151634728472509, 13.13951335195213233, 0.4288176399958442686 ) ) ;
#1846 = CIRCLE ( 'NONE', #12107, 11.02160133116777985 ) ;
#1847 = DIRECTION ( 'NONE',  ( 0.000000000000000000, 1.000000000000000000, 0.000000000000000000 ) ) ;
#1848 = CIRCLE ( 'NONE', #9980, 1.190625000000000711 ) ;
#1849 = ORIENTED_EDGE ( 'NONE', *, *, #11024, .F. ) ;
#1850 = CARTESIAN_POINT ( 'NONE',  ( 61.81956123787853130, 32.54502000000000095, -1.238102447480925239 ) ) ;
#1851 = DIRECTION ( 'NONE',  ( -0.6744690509234934073, -0.7360996206939023345, 0.05699866455150641442 ) ) ;
#1852 = SURFACE_STYLE_USAGE ( .BOTH. , #8477 ) ;
#1854 = CARTESIAN_POINT ( 'NONE',  ( 12.37528884409636021, -5.524115550796262042, -15.59548877588442650 ) ) ;
#1853 = DIRECTION ( 'NONE',  ( 0.000000000000000000, -1.000000000000000000, -0.000000000000000000 ) ) ;
#1855 = ORIENTED_EDGE ( 'NONE', *, *, #11172, .T. ) ;
#1856 = VERTEX_POINT ( 'NONE', #19308 ) ;
#1857 = CARTESIAN_POINT ( 'NONE',  ( 9.094193234406278137, 13.35316387417510242, 6.359510078786708931 ) ) ;
#1859 = CARTESIAN_POINT ( 'NONE',  ( -29.36874999999999858, 0.000000000000000000, 8.731885000000000119 ) ) ;
#1858 = CARTESIAN_POINT ( 'NONE',  ( 6.019117752002316912, 11.27437957348430153, 1.137765012461108727 ) ) ;
#1860 = ORIENTED_EDGE ( 'NONE', *, *, #496, .F. ) ;
#1861 = AXIS2_PLACEMENT_3D ( 'NONE', #3512, #21650, #10140 ) ;
#1862 = EDGE_LOOP ( 'NONE', ( #20036, #17938, #15260, #18256 ) ) ;
#1863 = EDGE_CURVE ( 'NONE', #11912, #13084, #7491, .T. ) ;
#1864 = DIRECTION ( 'NONE',  ( -0.8609107660235848503, 0.000000000000000000, 0.5087559856598096175 ) ) ;
#1865 = EDGE_LOOP ( 'NONE', ( #727, #19010, #8001, #1904 ) ) ;
#1866 = CARTESIAN_POINT ( 'NONE',  ( 7.485261295460871267, 16.46636833195797323, -2.127643011693920894 ) ) ;
#1867 = AXIS2_PLACEMENT_3D ( 'NONE', #3956, #8024, #7701 ) ;
#1868 = CARTESIAN_POINT ( 'NONE',  ( 54.55586098912687731, -1.983739999999999837, -6.056925149195119040 ) ) ;
#1869 = CARTESIAN_POINT ( 'NONE',  ( 2.520748753591570690, 102.1610225000000014, -24.56335908395234924 ) ) ;
#1870 = CARTESIAN_POINT ( 'NONE',  ( -0.08963606460140813303, 17.11798323789379239, 0.09094961474301116455 ) ) ;
#1871 = ORIENTED_EDGE ( 'NONE', *, *, #10172, .F. ) ;
#1872 = CARTESIAN_POINT ( 'NONE',  ( 2.799714621286362171, 11.92572550326888070, 3.472117233931273805 ) ) ;
#1873 = CARTESIAN_POINT ( 'NONE',  ( 61.02111788801703085, 0.000000000000000000, -5.406220493519755088 ) ) ;
#1874 = CARTESIAN_POINT ( 'NONE',  ( -3.042350287543033716, 3.961447500000001565, -26.17378113315171007 ) ) ;
#1875 = DIRECTION ( 'NONE',  ( 0.000000000000000000, 1.000000000000000000, 0.000000000000000000 ) ) ;
#1876 = VERTEX_POINT ( 'NONE', #4170 ) ;
#1877 = CARTESIAN_POINT ( 'NONE',  ( 8.904586033696963554, 18.52979832374122182, 7.665090501505551934 ) ) ;
#1878 = VECTOR ( 'NONE', #13860, 1000.000000000000000 ) ;
#1879 = CARTESIAN_POINT ( 'NONE',  ( 39.07078961959606289, -1.983739999999999837, -27.14892015257980162 ) ) ;
#1880 = CARTESIAN_POINT ( 'NONE',  ( 12.56049810209382578, 20.55707369507660687, 5.409390963554637111 ) ) ;
#1881 = ORIENTED_EDGE ( 'NONE', *, *, #4165, .T. ) ;
#1882 = ORIENTED_EDGE ( 'NONE', *, *, #3188, .T. ) ;
#1883 = EDGE_CURVE ( 'NONE', #20529, #15912, #413, .T. ) ;
#1884 = CARTESIAN_POINT ( 'NONE',  ( -6.268352501591477832, -7.547927499999999235, -35.49402737582407497 ) ) ;
#1885 = CARTESIAN_POINT ( 'NONE',  ( 8.906453209518582881, 11.27159611284453078, 4.875366572814009203 ) ) ;
#1886 = CARTESIAN_POINT ( 'NONE',  ( 5.411841742863021665, 15.73786965665290793, 8.085039117809539988 ) ) ;
#1887 = FACE_OUTER_BOUND ( 'NONE', #6145, .T. ) ;
#1888 = CARTESIAN_POINT ( 'NONE',  ( 6.124911956022416781, 11.96954057703546148, 1.636852048146504313 ) ) ;
#1889 = AXIS2_PLACEMENT_3D ( 'NONE', #2423, #7065, #12269 ) ;
#1890 = DIRECTION ( 'NONE',  ( 0.2064631973582987667, 0.000000000000000000, -0.9784543669157944601 ) ) ;
#1891 = EDGE_CURVE ( 'NONE', #21568, #12583, #7167, .T. ) ;
#1892 = CARTESIAN_POINT ( 'NONE',  ( 7.966291526427072611, 18.22263143684711650, -2.425212026461652126 ) ) ;
#1893 = CIRCLE ( 'NONE', #8262, 3.175000000000000711 ) ;
#1894 = CARTESIAN_POINT ( 'NONE',  ( 2.456256303170528899, 20.82653447492750232, 6.630392102736424320 ) ) ;
#1895 = CARTESIAN_POINT ( 'NONE',  ( -20.63749999999999929, 16.27314499999999953, 8.731249999999999289 ) ) ;
#1896 = PLANE ( 'NONE',  #9972 ) ;
#1897 = CARTESIAN_POINT ( 'NONE',  ( 1.044675250455524562, 12.39565097329668042, 6.288947036086600662 ) ) ;
#1898 = DIRECTION ( 'NONE',  ( 0.000000000000000000, -1.000000000000000000, 0.000000000000000000 ) ) ;
#1899 = CARTESIAN_POINT ( 'NONE',  ( 10.88641682560997204, -1.671568469779255439, -17.03366785910728964 ) ) ;
#1900 = AXIS2_PLACEMENT_3D ( 'NONE', #18001, #14482, #6058 ) ;
#1901 = CYLINDRICAL_SURFACE ( 'NONE', #4345, 0.5080000000000023386 ) ;
#1902 = CARTESIAN_POINT ( 'NONE',  ( 11.29248933744070094, 17.61190850482638126, 7.438500274146146118 ) ) ;
#1903 = DIRECTION ( 'NONE',  ( 0.000000000000000000, 1.000000000000000000, 0.000000000000000000 ) ) ;
#1904 = ORIENTED_EDGE ( 'NONE', *, *, #10523, .T. ) ;
#1905 = EDGE_CURVE ( 'NONE', #8949, #6182, #17556, .T. ) ;
#1906 = CARTESIAN_POINT ( 'NONE',  ( 11.37084557258393680, 12.66814131563982748, -2.073203632157150977 ) ) ;
#1907 = EDGE_CURVE ( 'NONE', #4938, #8453, #17059, .T. ) ;
#1908 = CARTESIAN_POINT ( 'NONE',  ( 6.585898268469219552, 1.984375000000000000, 4.694966092919240275 ) ) ;
#1910 = LINE ( 'NONE', #1689, #10939 ) ;
#1909 = CARTESIAN_POINT ( 'NONE',  ( 5.901153730144788057, 20.52421269917602231, 5.344389719742077105 ) ) ;
#1911 = CIRCLE ( 'NONE', #11461, 0.7950200000000003930 ) ;
#1912 = ORIENTED_EDGE ( 'NONE', *, *, #1404, .T. ) ;
#1913 = PLANE ( 'NONE',  #18047 ) ;
#1914 = CARTESIAN_POINT ( 'NONE',  ( 54.55586098912687731, -9.531985000000000596, -6.056925149195119040 ) ) ;
#1915 = DIRECTION ( 'NONE',  ( 0.05085730733808393328, 0.000000000000000000, -0.9987059298363656357 ) ) ;
#1916 = AXIS2_PLACEMENT_3D ( 'NONE', #7858, #11283, #4544 ) ;
#1917 = ORIENTED_EDGE ( 'NONE', *, *, #6375, .F. ) ;
#1918 = CARTESIAN_POINT ( 'NONE',  ( 8.565727124014848926, 11.53726303284714128, 3.541620658823112944 ) ) ;
#1919 = CARTESIAN_POINT ( 'NONE',  ( 3.468174865916350047, 20.55352757937665231, 3.625693982640088020 ) ) ;
#1920 = CARTESIAN_POINT ( 'NONE',  ( 13.94037765912086968, 20.92783617524978013, 3.342340119663654630 ) ) ;
#1921 = CARTESIAN_POINT ( 'NONE',  ( -0.4116026285172821320, 20.72700438578640458, 3.664095157482434306 ) ) ;
#1922 = CARTESIAN_POINT ( 'NONE',  ( 10.89765286091802210, 14.15736234249478720, -4.058299758797063284 ) ) ;
#1923 = CYLINDRICAL_SURFACE ( 'NONE', #18506, 0.7950200000000003930 ) ;
#1924 = EDGE_CURVE ( 'NONE', #19794, #14117, #13931, .T. ) ;
#1925 = CARTESIAN_POINT ( 'NONE',  ( 12.99564195812022405, -0.1559143132144474864, -16.39129925056700543 ) ) ;
#1926 = UNCERTAINTY_MEASURE_WITH_UNIT (LENGTH_MEASURE( 1.000000000000000082E-05 ), #12674, 'distance_accuracy_value', 'NONE');
#1927 = CARTESIAN_POINT ( 'NONE',  ( 52.96420052373725440, 0.000000000000000000, 7.017842122255405712 ) ) ;
#1928 = ORIENTED_EDGE ( 'NONE', *, *, #13864, .F. ) ;
#1929 = CARTESIAN_POINT ( 'NONE',  ( 11.19880827645247479, 14.32817945148129191, 6.410845832078652329 ) ) ;
#1930 = CARTESIAN_POINT ( 'NONE',  ( 7.454783155005726414, 18.37230293632699230, -2.665002534372324039 ) ) ;
#1931 = ORIENTED_EDGE ( 'NONE', *, *, #21706, .T. ) ;
#1932 = EDGE_CURVE ( 'NONE', #19840, #9986, #12584, .T. ) ;
#1933 = CARTESIAN_POINT ( 'NONE',  ( 46.03750000000000142, 42.06303499999999929, -10.31874999999999964 ) ) ;
#1934 = DIRECTION ( 'NONE',  ( -0.4857267349359786768, 0.000000000000000000, 0.8741107132214052111 ) ) ;
#1935 = EDGE_CURVE ( 'NONE', #19764, #15380, #18870, .T. ) ;
#1937 = DIRECTION ( 'NONE',  ( -0.2490110332224836354, 0.000000000000000000, 0.9685006480810794960 ) ) ;
#1936 = CARTESIAN_POINT ( 'NONE',  ( 6.183449657823808288, 10.85153064243760213, 2.375645654555686104 ) ) ;
#1938 = ORIENTED_EDGE ( 'NONE', *, *, #10853, .F. ) ;
#1939 = CARTESIAN_POINT ( 'NONE',  ( 7.545109171398233450, 14.90330900736333142, 8.204851733050276152 ) ) ;
#1940 = EDGE_LOOP ( 'NONE', ( #14741, #1746, #6135, #11189 ) ) ;
#1941 = DIRECTION ( 'NONE',  ( 0.000000000000000000, 1.000000000000000000, 0.000000000000000000 ) ) ;
#1942 = ORIENTED_EDGE ( 'NONE', *, *, #3071, .T. ) ;
#1943 = CARTESIAN_POINT ( 'NONE',  ( 1.885017549903653888, 14.91461614480940945, 0.3181462793239871467 ) ) ;
#1944 = AXIS2_PLACEMENT_3D ( 'NONE', #14933, #11374, #7828 ) ;
#1945 = CARTESIAN_POINT ( 'NONE',  ( 3.766360634439569033, 14.28061422378609002, -0.1577300086709537419 ) ) ;
#1946 = FACE_OUTER_BOUND ( 'NONE', #5301, .T. ) ;
#1947 = DIRECTION ( 'NONE',  ( 0.000000000000000000, -1.000000000000000000, -0.000000000000000000 ) ) ;
#1948 = EDGE_CURVE ( 'NONE', #17792, #1329, #7039, .T. ) ;
#1949 = LINE ( 'NONE', #11588, #21721 ) ;
#1950 = CARTESIAN_POINT ( 'NONE',  ( 4.620631840053190942, 20.50352216405097749, 6.712139773280671129 ) ) ;
#1951 = EDGE_CURVE ( 'NONE', #19608, #17559, #9133, .T. ) ;
#1952 = CARTESIAN_POINT ( 'NONE',  ( 23.77193158452286781, 28.96330250000000461, -15.00033089984030887 ) ) ;
#1953 = EDGE_CURVE ( 'NONE', #7817, #3064, #9657, .T. ) ;
#1954 = ORIENTED_EDGE ( 'NONE', *, *, #11915, .F. ) ;
#1955 = CARTESIAN_POINT ( 'NONE',  ( 38.82016491058538321, 34.52875999999999834, -14.75770094105646812 ) ) ;
#1956 = DIRECTION ( 'NONE',  ( 0.000000000000000000, 1.000000000000000000, 0.000000000000000000 ) ) ;
#1957 = DIRECTION ( 'NONE',  ( 0.2490110332224850509, 0.000000000000000000, -0.9685006480810792739 ) ) ;
#1958 = CARTESIAN_POINT ( 'NONE',  ( 26.59062499999999929, 2.380615000000000148, 8.731249999999999289 ) ) ;
#1960 = CARTESIAN_POINT ( 'NONE',  ( 13.22923918826351297, -6.405949669792143197, -15.43418026626714301 ) ) ;
#1959 = DIRECTION ( 'NONE',  ( 0.000000000000000000, 1.000000000000000000, 0.000000000000000000 ) ) ;
#1961 = ORIENTED_EDGE ( 'NONE', *, *, #6404, .T. ) ;
#1962 = ORIENTED_EDGE ( 'NONE', *, *, #7537, .T. ) ;
#1963 = CARTESIAN_POINT ( 'NONE',  ( 9.285644904300696112, 17.21895884409014599, -2.864567016515628062 ) ) ;
#1965 = DIRECTION ( 'NONE',  ( 0.000000000000000000, -1.000000000000000000, -0.000000000000000000 ) ) ;
#1964 = CARTESIAN_POINT ( 'NONE',  ( 3.701753992781950053, 14.72343274211524644, 9.049335738697640963 ) ) ;
#1966 = VERTEX_POINT ( 'NONE', #15473 ) ;
#1967 = CARTESIAN_POINT ( 'NONE',  ( 5.516318909232666101, 16.92504161144799468, 8.771371271385028479 ) ) ;
#1968 = VERTEX_POINT ( 'NONE', #9028 ) ;
#1969 = CARTESIAN_POINT ( 'NONE',  ( 60.38511073144201191, -1.983739999999999837, -22.26373525985038526 ) ) ;
#1970 = EDGE_LOOP ( 'NONE', ( #13062, #3651, #5071, #11243 ) ) ;
#1971 = CARTESIAN_POINT ( 'NONE',  ( 7.521333489489228086, 16.89536166212861090, -2.106288691737336016 ) ) ;
#1972 = LINE ( 'NONE', #15490, #17384 ) ;
#1973 = ORIENTED_EDGE ( 'NONE', *, *, #9073, .T. ) ;
#1974 = CARTESIAN_POINT ( 'NONE',  ( 3.426769813837023282, 14.84877425439436571, 8.187781101960947439 ) ) ;
#1975 = ADVANCED_FACE ( 'NONE', ( #3738 ), #629, .F. ) ;
#1976 = CARTESIAN_POINT ( 'NONE',  ( 59.55063415577301811, 34.52875999999999834, -22.52230776719629191 ) ) ;
#1977 = DIRECTION ( 'NONE',  ( 0.000000000000000000, 0.000000000000000000, -1.000000000000000000 ) ) ;
#1978 = CARTESIAN_POINT ( 'NONE',  ( 3.190248314799053464, 19.04062286170201546, 8.431111234986099490 ) ) ;
#1979 = EDGE_CURVE ( 'NONE', #12265, #10693, #1189, .T. ) ;
#1980 = CYLINDRICAL_SURFACE ( 'NONE', #5566, 8.929687500000001776 ) ;
#1981 = VERTEX_POINT ( 'NONE', #15914 ) ;
#1982 = CARTESIAN_POINT ( 'NONE',  ( 3.721838304568709344, 16.48662853297856401, 8.524029460627765786 ) ) ;
#1983 = DIRECTION ( 'NONE',  ( -0.6702301885068632226, 0.000000000000000000, -0.7421532822901576454 ) ) ;
#1984 = CARTESIAN_POINT ( 'NONE',  ( 52.89469146228504570, -5.197312526642835273, -16.93126689015821640 ) ) ;
#1985 = DIRECTION ( 'NONE',  ( 0.9636276526537417286, 0.000000000000000000, -0.2672484743474500268 ) ) ;
#1986 = ORIENTED_EDGE ( 'NONE', *, *, #8283, .F. ) ;
#1987 = CARTESIAN_POINT ( 'NONE',  ( 5.982655683593218754, 20.62467454825192092, -0.1193919904210567484 ) ) ;
#1988 = DIRECTION ( 'NONE',  ( -0.9964481331860212121, 0.000000000000000000, 0.08420877549337302259 ) ) ;
#1989 = CARTESIAN_POINT ( 'NONE',  ( 11.95762566148904327, 21.63633082368178151, 3.785239628339895912 ) ) ;
#1990 = VERTEX_POINT ( 'NONE', #525 ) ;
#1991 = ORIENTED_EDGE ( 'NONE', *, *, #5836, .T. ) ;
#1992 = DIRECTION ( 'NONE',  ( 0.2227372614607789347, 0.000000000000000000, 0.9748785115884710528 ) ) ;
#1993 = CARTESIAN_POINT ( 'NONE',  ( 9.441105179033391082, 16.62352861847284657, 7.978075225639419621 ) ) ;
#1994 = CARTESIAN_POINT ( 'NONE',  ( 1.524583137339517780, 15.70105570582070520, 8.880780227086491507 ) ) ;
#1995 = CARTESIAN_POINT ( 'NONE',  ( 6.138121642458962413, 19.25141403178904298, -0.4363714260734747330 ) ) ;
#1996 = CARTESIAN_POINT ( 'NONE',  ( 7.048998319408883440, 18.08802919812652021, 7.290918307196334602 ) ) ;
#1997 = FACE_OUTER_BOUND ( 'NONE', #4358, .T. ) ;
#1998 = VECTOR ( 'NONE', #9440, 1000.000000000000000 ) ;
#1999 = CARTESIAN_POINT ( 'NONE',  ( 7.539145179894531701, 16.37851731477712391, -3.008003415082166399 ) ) ;
#2000 = CARTESIAN_POINT ( 'NONE',  ( -0.7351689855894368852, 20.80871142581116118, 3.732510512736133546 ) ) ;
#2001 = CARTESIAN_POINT ( 'NONE',  ( 0.6418754216142991131, 20.43628740585238646, 7.348520308371068843 ) ) ;
#2002 = EDGE_CURVE ( 'NONE', #16776, #7796, #14035, .T. ) ;
#2003 = CARTESIAN_POINT ( 'NONE',  ( 38.23013820809905638, 109.3223030719999969, -14.22485453658974031 ) ) ;
#2004 = CARTESIAN_POINT ( 'NONE',  ( 1.450916895402551532, 14.30666394527731633, 8.434575071336105623 ) ) ;
#2005 = FACE_OUTER_BOUND ( 'NONE', #18425, .T. ) ;
#2006 = CARTESIAN_POINT ( 'NONE',  ( 17.44897684999575915, -8.217241507614266638, -15.76094700865116138 ) ) ;
#2007 = DIRECTION ( 'NONE',  ( 0.2490110332224846623, 0.000000000000000000, -0.9685006480810793850 ) ) ;
#2008 = DIRECTION ( 'NONE',  ( 0.6702301885068638887, 0.000000000000000000, 0.7421532822901570903 ) ) ;
#2009 = CARTESIAN_POINT ( 'NONE',  ( 11.39633395548191785, 16.56875889582252270, 7.579279425343053767 ) ) ;
#2010 = DIRECTION ( 'NONE',  ( 0.7421532822901569793, 0.000000000000000000, -0.6702301885068642218 ) ) ;
#2011 = CARTESIAN_POINT ( 'NONE',  ( 11.36068676796085875, 17.98270986927288106, -3.346212262616973021 ) ) ;
#2012 = CARTESIAN_POINT ( 'NONE',  ( 12.46399079089267836, -5.664758814889668592, -16.85385019909982418 ) ) ;
#2013 = CARTESIAN_POINT ( 'NONE',  ( 3.722424747480308493, 20.61711312421807918, 5.170631176151997188 ) ) ;
#2014 = ORIENTED_EDGE ( 'NONE', *, *, #1415, .F. ) ;
#2015 = APPLICATION_PROTOCOL_DEFINITION ( 'draft international standard', 'automotive_design', 1998, #12720 ) ;
#2016 = DIRECTION ( 'NONE',  ( 0.000000000000000000, 1.000000000000000000, 0.000000000000000000 ) ) ;
#2017 = CARTESIAN_POINT ( 'NONE',  ( 4.241210656867956175, 19.03653144147999754, 0.1777686537783049470 ) ) ;
#2018 = B_SPLINE_CURVE_WITH_KNOTS ( 'NONE', 3,
 ( #546, #8824, #7189, #18994, #3871, #10608, #17357, #8941, #14712, #1198 ),
 .UNSPECIFIED., .F., .F.,
 ( 4, 2, 2, 2, 4 ),
 ( 0.006416468533192019007, 0.006892176379334203663, 0.007367884225476389187, 0.007843592071618573844, 0.008319299917760758500 ),
 .UNSPECIFIED. ) ;
#2019 = DIRECTION ( 'NONE',  ( 0.2490110332224850509, 0.000000000000000000, -0.9685006480810792739 ) ) ;
#2020 = VERTEX_POINT ( 'NONE', #20740 ) ;
#2021 = CARTESIAN_POINT ( 'NONE',  ( 11.10449564925248467, 12.61980174807018251, 5.312955716968204456 ) ) ;
#2022 = CARTESIAN_POINT ( 'NONE',  ( 9.316180898295447932, 14.88029421051436429, 7.101556370160515996 ) ) ;
#2023 = CARTESIAN_POINT ( 'NONE',  ( 7.188422006453914825, 19.80783775455006435, 6.631232769852104525 ) ) ;
#2024 = CARTESIAN_POINT ( 'NONE',  ( 10.75667203142358019, 10.89927089225536250, 4.183043474010283980 ) ) ;
#2025 = EDGE_CURVE ( 'NONE', #1512, #9499, #10357, .T. ) ;
#2026 = AXIS2_PLACEMENT_3D ( 'NONE', #18346, #3213, #1549 ) ;
#2027 = DIRECTION ( 'NONE',  ( 1.000000000000000000, 0.000000000000000000, 0.000000000000000000 ) ) ;
#2028 = CARTESIAN_POINT ( 'NONE',  ( 18.79169812173498144, -0.2733990383971263149, -14.58197954317160416 ) ) ;
#2029 = CARTESIAN_POINT ( 'NONE',  ( 11.67873622359053165, -4.444366717925562149, -15.39547690709331995 ) ) ;
#2030 = VERTEX_POINT ( 'NONE', #12359 ) ;
#2031 = CARTESIAN_POINT ( 'NONE',  ( 11.51558075932182845, 10.98646219477360297, -1.335441368411448115 ) ) ;
#2032 = ORIENTED_EDGE ( 'NONE', *, *, #19528, .F. ) ;
#2033 = CARTESIAN_POINT ( 'NONE',  ( 9.643416883055870414, 12.23232111864449756, -0.7319516263326404371 ) ) ;
#2034 = DIRECTION ( 'NONE',  ( 0.000000000000000000, -1.000000000000000000, 0.000000000000000000 ) ) ;
#2035 = CARTESIAN_POINT ( 'NONE',  ( 13.30756833192837973, 22.19916104524133971, 1.697755270691982732 ) ) ;
#2037 = DIRECTION ( 'NONE',  ( -0.9579671649362032637, 0.000000000000000000, 0.2868778675745010664 ) ) ;
#2036 = CARTESIAN_POINT ( 'NONE',  ( 1.396283581706163179, 16.44430802189885199, -0.6243410038125684069 ) ) ;
#2038 = ORIENTED_EDGE ( 'NONE', *, *, #2764, .T. ) ;
#2039 = CARTESIAN_POINT ( 'NONE',  ( 7.397026236728797777, 12.98560518583070156, 7.265883842775997081 ) ) ;
#2040 = DIRECTION ( 'NONE',  ( 0.6744690509234934073, 0.7360996206939024455, -0.05699866455150642136 ) ) ;
#2041 = VECTOR ( 'NONE', #20727, 1000.000000000000227 ) ;
#2042 = ORIENTED_EDGE ( 'NONE', *, *, #14952, .T. ) ;
#2043 = ADVANCED_FACE ( 'NONE', ( #19085 ), #17446, .F. ) ;
#2044 = CARTESIAN_POINT ( 'NONE',  ( 0.04798837220721437896, 15.99000724392452355, 0.8174092256989702321 ) ) ;
#2045 = CARTESIAN_POINT ( 'NONE',  ( -22.33576604192310455, 5.149960319306146062E-16, 0.9319226134156144425 ) ) ;
#2046 = ORIENTED_EDGE ( 'NONE', *, *, #21118, .T. ) ;
#2047 = EDGE_CURVE ( 'NONE', #18768, #2822, #14695, .T. ) ;
#2048 = CARTESIAN_POINT ( 'NONE',  ( 3.931607425614295881, 13.02331082334462664, 0.7891442226006756266 ) ) ;
#2049 = ADVANCED_FACE ( 'NONE', ( #1284 ), #11349, .T. ) ;
#2050 = EDGE_CURVE ( 'NONE', #21656, #4533, #12134, .T. ) ;
#2051 = CARTESIAN_POINT ( 'NONE',  ( -29.36874999999999858, 30.56128000000000000, 10.71562499999999929 ) ) ;
#2052 = CARTESIAN_POINT ( 'NONE',  ( 55.27198911326564001, 0.000000000000000000, 2.462719476673013830 ) ) ;
#2053 = CARTESIAN_POINT ( 'NONE',  ( 0.02083138522551555155, 12.30439499999999953, 7.210477125664100484 ) ) ;
#2054 = CARTESIAN_POINT ( 'NONE',  ( 5.075214630907313840, 19.34300442968084965, 7.864654554335390735 ) ) ;
#2055 = CARTESIAN_POINT ( 'NONE',  ( 1.402240371799016394, 9.120973559619994120, 10.67764259629631951 ) ) ;
#2056 = AXIS2_PLACEMENT_3D ( 'NONE', #11844, #18251, #3220 ) ;
#2057 = EDGE_LOOP ( 'NONE', ( #21720, #14710, #21033, #18291 ) ) ;
#2058 = DIRECTION ( 'NONE',  ( 0.000000000000000000, -1.000000000000000000, -0.000000000000000000 ) ) ;
#2059 = CYLINDRICAL_SURFACE ( 'NONE', #20534, 30.16249999999999076 ) ;
#2060 = SURFACE_STYLE_FILL_AREA ( #18872 ) ;
#2062 = CARTESIAN_POINT ( 'NONE',  ( 19.41812612159816354, -4.815725606720878460, -14.19246007111251551 ) ) ;
#2061 = DIRECTION ( 'NONE',  ( 0.5087559856598092844, 0.000000000000000000, 0.8609107660235849613 ) ) ;
#2063 = ORIENTED_EDGE ( 'NONE', *, *, #15564, .F. ) ;
#2064 = ORIENTED_EDGE ( 'NONE', *, *, #15467, .F. ) ;
#2065 = CARTESIAN_POINT ( 'NONE',  ( 11.63657489771697762, 19.71324643990528358, -2.510315654606890767 ) ) ;
#2067 = DIRECTION ( 'NONE',  ( -0.9161599507719021540, -0.3242921320961419940, -0.2355537256384720723 ) ) ;
#2066 = CARTESIAN_POINT ( 'NONE',  ( 1.666480301802111708, 14.62668795976242642, -0.5087735202898915343 ) ) ;
#2068 = ORIENTED_EDGE ( 'NONE', *, *, #11302, .T. ) ;
#2070 = CARTESIAN_POINT ( 'NONE',  ( 14.59416852906185902, -8.664514012370643670, -15.20522331642918168 ) ) ;
#2069 = CARTESIAN_POINT ( 'NONE',  ( 4.428162769058000769, 11.10825873668719233, 3.140058628108473027 ) ) ;
#2071 = ORIENTED_EDGE ( 'NONE', *, *, #14354, .F. ) ;
#2072 = ORIENTED_EDGE ( 'NONE', *, *, #14472, .F. ) ;
#2073 = EDGE_CURVE ( 'NONE', #18658, #16568, #9570, .T. ) ;
#2074 = CARTESIAN_POINT ( 'NONE',  ( 7.974225380408622499, 19.27095890255583654, -1.194036445722556294 ) ) ;
#2075 = CARTESIAN_POINT ( 'NONE',  ( 12.91596452321051558, 20.23395749999999893, 2.799331278665067479 ) ) ;
#2076 = CIRCLE ( 'NONE', #7372, 3.968750000000000000 ) ;
#2077 = ORIENTED_EDGE ( 'NONE', *, *, #5527, .F. ) ;
#2078 = EDGE_CURVE ( 'NONE', #21155, #5628, #13555, .T. ) ;
#2079 = DIRECTION ( 'NONE',  ( 0.000000000000000000, 0.000000000000000000, -1.000000000000000000 ) ) ;
#2080 = EDGE_CURVE ( 'NONE', #3371, #8815, #17439, .T. ) ;
#2081 = CARTESIAN_POINT ( 'NONE',  ( 17.77223365658175069, 0.4543760498246959822, 9.996193404372801794 ) ) ;
#2082 = CIRCLE ( 'NONE', #15531, 0.7950200000000000600 ) ;
#2083 = DIRECTION ( 'NONE',  ( -0.7421532822901579785, 0.000000000000000000, 0.6702301885068628895 ) ) ;
#2084 = DIRECTION ( 'NONE',  ( 0.4987171968201928873, 0.000000000000000000, -0.8667647648559606566 ) ) ;
#2085 = FACE_OUTER_BOUND ( 'NONE', #10972, .T. ) ;
#2086 = CARTESIAN_POINT ( 'NONE',  ( 2.034095840400902411, 21.12497993269252206, 5.441157602331140097 ) ) ;
#2087 = LINE ( 'NONE', #20216, #11922 ) ;
#2088 = ORIENTED_EDGE ( 'NONE', *, *, #17214, .T. ) ;
#2089 = CARTESIAN_POINT ( 'NONE',  ( -3.246390552019219999, 12.30439499999999953, 3.217431771123079987 ) ) ;
#2090 = LINE ( 'NONE', #20320, #5341 ) ;
#2091 = LINE ( 'NONE', #10831, #6773 ) ;
#2092 = ORIENTED_EDGE ( 'NONE', *, *, #11972, .F. ) ;
#2093 = CARTESIAN_POINT ( 'NONE',  ( 11.71175349776414798, 21.61111399576532222, 4.019351335416992299 ) ) ;
#2094 = DIRECTION ( 'NONE',  ( 0.9685006480810792739, 0.000000000000000000, 0.2490110332224846346 ) ) ;
#2095 = CARTESIAN_POINT ( 'NONE',  ( 11.07300705963626086, 22.03001829576734139, 1.335942992242750815 ) ) ;
#2096 = VERTEX_POINT ( 'NONE', #9357 ) ;
#2097 = ORIENTED_EDGE ( 'NONE', *, *, #203, .F. ) ;
#2098 = CARTESIAN_POINT ( 'NONE',  ( 13.19949732976186674, 21.42485117465795241, 1.390320667582642278 ) ) ;
#2099 = CARTESIAN_POINT ( 'NONE',  ( 9.353409075422060681, 13.00170194491951747, 6.914035789133324172 ) ) ;
#2100 = CARTESIAN_POINT ( 'NONE',  ( 3.774570344757517404, 14.05232170482083198, -0.1440267703289939694 ) ) ;
#2101 = CARTESIAN_POINT ( 'NONE',  ( 49.79678389823170903, 0.000000000000000000, -28.13445659451038594 ) ) ;
#2102 = AXIS2_PLACEMENT_3D ( 'NONE', #9867, #14883, #3257 ) ;
#2103 = ADVANCED_FACE ( 'NONE', ( #21401 ), #21508, .T. ) ;
#2104 = VECTOR ( 'NONE', #791, 1000.000000000000114 ) ;
#2105 = CARTESIAN_POINT ( 'NONE',  ( 5.828491125658624483, 12.77629345597859611, 0.2544156256959317353 ) ) ;
#2106 = CARTESIAN_POINT ( 'NONE',  ( 7.278394972475737745, 16.40995809457478316, 7.634184181800698354 ) ) ;
#2107 = EDGE_CURVE ( 'NONE', #3226, #2636, #18100, .T. ) ;
#2108 = EDGE_CURVE ( 'NONE', #10320, #2958, #18819, .T. ) ;
#2109 = DIRECTION ( 'NONE',  ( 0.9964481331860213231, 0.000000000000000000, -0.08420877549337293932 ) ) ;
#2110 = AXIS2_PLACEMENT_3D ( 'NONE', #16637, #18498, #12100 ) ;
#2111 = CARTESIAN_POINT ( 'NONE',  ( 12.05982911834764160, 19.98250042233096124, -2.959000471914774888 ) ) ;
#2112 =( REPRESENTATION_RELATIONSHIP ('NONE','NONE', #15554, #21464 ) REPRESENTATION_RELATIONSHIP_WITH_TRANSFORMATION ( #7875 )SHAPE_REPRESENTATION_RELATIONSHIP( ) );
#2113 = DIRECTION ( 'NONE',  ( 0.000000000000000000, 1.000000000000000000, 0.000000000000000000 ) ) ;
#2114 = CARTESIAN_POINT ( 'NONE',  ( 6.375721097596529496, 21.18628736811522373, 5.516090907968282053 ) ) ;
#2115 = CARTESIAN_POINT ( 'NONE',  ( -0.02957876527916961790, 21.01733645358232039, 5.567338713754919510 ) ) ;
#2116 = CARTESIAN_POINT ( 'NONE',  ( 19.83642166017488151, -0.1294698813808727589, -14.85952381701978453 ) ) ;
#2117 = CIRCLE ( 'NONE', #12729, 1.190625000000000711 ) ;
#2118 = CARTESIAN_POINT ( 'NONE',  ( 3.381061492508358413, 16.48226916726223479, 8.534974189403024880 ) ) ;
#2119 = CARTESIAN_POINT ( 'NONE',  ( 29.64606458365116737, 34.51447250000000366, -15.53894806404596096 ) ) ;
#2120 = CYLINDRICAL_SURFACE ( 'NONE', #3730, 0.5079999999999984528 ) ;
#2121 = CARTESIAN_POINT ( 'NONE',  ( 11.96169894293330138, 0.4392826198422947193, -16.66899426637521842 ) ) ;
#2122 = VECTOR ( 'NONE', #827, 1000.000000000000000 ) ;
#2123 = SURFACE_STYLE_FILL_AREA ( #17054 ) ;
#2124 = CARTESIAN_POINT ( 'NONE',  ( 10.91865587142655158, 19.54907707356796109, 6.609524152570670275 ) ) ;
#2125 = CARTESIAN_POINT ( 'NONE',  ( 29.64606458365116737, -6.752907499999998286, -15.53894806404596096 ) ) ;
#2126 = CARTESIAN_POINT ( 'NONE',  ( 11.15127959100651722, 15.67546746552279302, -3.541987318106106120 ) ) ;
#2127 = AXIS2_PLACEMENT_3D ( 'NONE', #12879, #11421, #1243 ) ;
#2128 = CARTESIAN_POINT ( 'NONE',  ( 61.83151161312219557, 34.52875999999999834, -0.3645647634491749334 ) ) ;
#2129 = ORIENTED_EDGE ( 'NONE', *, *, #10973, .F. ) ;
#2130 = APPLICATION_PROTOCOL_DEFINITION ( 'draft international standard', 'automotive_design', 1998, #10749 ) ;
#2131 = FILL_AREA_STYLE ('',( #8988 ) ) ;
#2132 = CARTESIAN_POINT ( 'NONE',  ( 4.996268568956748091, 20.49501342957312744, 2.074042226353195684 ) ) ;
#2133 = ADVANCED_FACE ( 'NONE', ( #19849 ), #953, .F. ) ;
#2134 = CIRCLE ( 'NONE', #7393, 3.175000000000001155 ) ;
#2135 = CARTESIAN_POINT ( 'NONE',  ( 52.91483696501514800, -5.165959288209053923, -16.50498455623153404 ) ) ;
#2136 = VECTOR ( 'NONE', #16627, 1000.000000000000000 ) ;
#2137 = ORIENTED_EDGE ( 'NONE', *, *, #16907, .F. ) ;
#2138 = CARTESIAN_POINT ( 'NONE',  ( 9.274993866748067362, 13.35316387417510242, 6.305366573914296779 ) ) ;
#2139 = STYLED_ITEM ( 'NONE', ( #10043 ), #5939 ) ;
#2140 = CARTESIAN_POINT ( 'NONE',  ( 7.475049925495288683, 16.36412484890493957, -2.235126692085353639 ) ) ;
#2141 = CARTESIAN_POINT ( 'NONE',  ( 0.5343612684300755866, 18.97471059823722328, 0.6418818272746593667 ) ) ;
#2142 = CARTESIAN_POINT ( 'NONE',  ( 13.28268573882264469, 19.39178765922512326, -19.83174211820151100 ) ) ;
#2143 = AXIS2_PLACEMENT_3D ( 'NONE', #7385, #7710, #14470 ) ;
#2144 = CARTESIAN_POINT ( 'NONE',  ( -17.46249999999999858, -1.587500000000002132, 0.000000000000000000 ) ) ;
#2145 = CARTESIAN_POINT ( 'NONE',  ( 16.67159889069950296, 1.010067806219507647, -15.24940416025467904 ) ) ;
#2146 = CARTESIAN_POINT ( 'NONE',  ( 65.51436440461340283, 0.000000000000000000, -12.87863775929475985 ) ) ;
#2147 = ORIENTED_EDGE ( 'NONE', *, *, #3587, .F. ) ;
#2148 = CARTESIAN_POINT ( 'NONE',  ( 6.283322441762637212, 20.69450185495974281, -0.2642756491526417895 ) ) ;
#2149 = MECHANICAL_DESIGN_GEOMETRIC_PRESENTATION_REPRESENTATION (  '', ( #11690 ), #18747 ) ;
#2150 = FACE_OUTER_BOUND ( 'NONE', #12578, .T. ) ;
#2151 = EDGE_LOOP ( 'NONE', ( #4488, #19389, #2830, #5520 ) ) ;
#2152 = CARTESIAN_POINT ( 'NONE',  ( 9.291847323842565842, 15.23045113553444097, -2.731355305102841413 ) ) ;
#2153 = PLANE ( 'NONE',  #1078 ) ;
#2154 = CARTESIAN_POINT ( 'NONE',  ( -17.46249999999999858, 33.73373999999999739, 0.000000000000000000 ) ) ;
#2156 = CARTESIAN_POINT ( 'NONE',  ( 35.15748561355322011, 0.000000000000000000, 0.3244898641346534163 ) ) ;
#2155 = CARTESIAN_POINT ( 'NONE',  ( 0.9545976637875654980, 21.03017768341116067, 3.424241316347047981 ) ) ;
#2157 = ORIENTED_EDGE ( 'NONE', *, *, #21610, .F. ) ;
#2158 = CARTESIAN_POINT ( 'NONE',  ( 7.541834703702306797, 14.74947482163050161, 8.160879108828842377 ) ) ;
#2159 = CIRCLE ( 'NONE', #15957, 0.7950199999999998379 ) ;
#2160 = ADVANCED_FACE ( 'NONE', ( #14464 ), #19532, .T. ) ;
#2161 = FACE_OUTER_BOUND ( 'NONE', #5062, .T. ) ;
#2162 = ORIENTED_EDGE ( 'NONE', *, *, #21483, .F. ) ;
#2163 = VECTOR ( 'NONE', #13334, 1000.000000000000114 ) ;
#2164 = DIRECTION ( 'NONE',  ( 0.2064631973582987667, 0.000000000000000000, -0.9784543669157944601 ) ) ;
#2165 = CIRCLE ( 'NONE', #14549, 1.983739999999999393 ) ;
#2166 = FACE_OUTER_BOUND ( 'NONE', #10801, .T. ) ;
#2167 = ORIENTED_EDGE ( 'NONE', *, *, #18913, .F. ) ;
#2168 = CARTESIAN_POINT ( 'NONE',  ( 2.651964239740473683, 19.43893749999999798, 5.873042593501262232 ) ) ;
#2169 = VECTOR ( 'NONE', #11187, 1000.000000000000114 ) ;
#2170 = CYLINDRICAL_SURFACE ( 'NONE', #16338, 15.47812499999999680 ) ;
#2171 = VECTOR ( 'NONE', #10766, 1000.000000000000000 ) ;
#2172 = FACE_OUTER_BOUND ( 'NONE', #5735, .T. ) ;
#2173 = CARTESIAN_POINT ( 'NONE',  ( 1.603642987080700744, 9.058787236897966721, 10.70057449157679663 ) ) ;
#2174 = CIRCLE ( 'NONE', #3588, 1.190625000000000711 ) ;
#2175 = CIRCLE ( 'NONE', #10306, 1.983739999999997616 ) ;
#2176 = ORIENTED_EDGE ( 'NONE', *, *, #12352, .F. ) ;
#2177 = CARTESIAN_POINT ( 'NONE',  ( 11.75439013559175017, 36.51313500000000545, 4.331204221326972359 ) ) ;
#2178 = CARTESIAN_POINT ( 'NONE',  ( 71.03963378001139972, 0.000000000000000000, -10.54138470677948014 ) ) ;
#2179 = CARTESIAN_POINT ( 'NONE',  ( 26.59062499999999929, 30.56064500000000095, 8.335010000000000474 ) ) ;
#2181 = CARTESIAN_POINT ( 'NONE',  ( 14.29938834594686448, -6.988883160487315394, -15.21728503260617593 ) ) ;
#2180 = CARTESIAN_POINT ( 'NONE',  ( 29.15193331460030279, 30.55334249999999940, -13.61707959051006966 ) ) ;
#2182 = EDGE_LOOP ( 'NONE', ( #7820, #21657, #6898, #18046 ) ) ;
#2183 = ORIENTED_EDGE ( 'NONE', *, *, #12051, .F. ) ;
#2184 = AXIS2_PLACEMENT_3D ( 'NONE', #5383, #7375, #5600 ) ;
#2185 = CARTESIAN_POINT ( 'NONE',  ( 12.78095741915561945, 21.47881914407666315, 0.5220334371899034709 ) ) ;
#2186 = AXIS2_PLACEMENT_3D ( 'NONE', #17579, #18897, #17365 ) ;
#2188 = LINE ( 'NONE', #17454, #18085 ) ;
#2187 = CARTESIAN_POINT ( 'NONE',  ( 5.179235369666963074, 19.21458830873230283, 8.065034840720384679 ) ) ;
#2189 = ORIENTED_EDGE ( 'NONE', *, *, #10352, .F. ) ;
#2191 = CARTESIAN_POINT ( 'NONE',  ( 21.25282423609957050, -2.645784314445630780, -13.67651348702517744 ) ) ;
#2190 = CARTESIAN_POINT ( 'NONE',  ( 5.543297571818101233, 13.82534514388550129, 8.177650472684211636 ) ) ;
#2192 = ORIENTED_EDGE ( 'NONE', *, *, #7383, .T. ) ;
#2193 = EDGE_CURVE ( 'NONE', #10898, #10146, #855, .T. ) ;
#2194 = ORIENTED_EDGE ( 'NONE', *, *, #20013, .F. ) ;
#2195 = ADVANCED_FACE ( 'NONE', ( #19411 ), #12809, .T. ) ;
#2196 = CARTESIAN_POINT ( 'NONE',  ( 7.609271008339460352, 13.06901655821814145, -0.8557159515761880719 ) ) ;
#2197 = VECTOR ( 'NONE', #14140, 1000.000000000000000 ) ;
#2198 = ORIENTED_EDGE ( 'NONE', *, *, #9674, .F. ) ;
#2199 = AXIS2_PLACEMENT_3D ( 'NONE', #2142, #14330, #703 ) ;
#2200 = DIRECTION ( 'NONE',  ( -0.2868778675745011220, 0.000000000000000000, -0.9579671649362034858 ) ) ;
#2201 = CARTESIAN_POINT ( 'NONE',  ( -17.16618386210371483, 39.44874000000000080, 58.07004290071009223 ) ) ;
#2202 = DIRECTION ( 'NONE',  ( 0.000000000000000000, 1.000000000000000000, 0.000000000000000000 ) ) ;
#2203 = CARTESIAN_POINT ( 'NONE',  ( 0.7633619320212706727, 20.37518500713720471, 2.043613188576509199 ) ) ;
#2204 = VERTEX_POINT ( 'NONE', #21073 ) ;
#2205 = CARTESIAN_POINT ( 'NONE',  ( 3.936278269025204501, 16.50247895544803711, 8.791069023109434610 ) ) ;
#2206 = CARTESIAN_POINT ( 'NONE',  ( 46.03750000000000142, -9.531985000000000596, -10.31874999999999964 ) ) ;
#2207 = CARTESIAN_POINT ( 'NONE',  ( 13.24246334734214336, 22.12989337480687269, 1.990192772094774076 ) ) ;
#2208 = ADVANCED_FACE ( 'NONE', ( #7808 ), #5924, .T. ) ;
#2209 = DIRECTION ( 'NONE',  ( 0.000000000000000000, -1.000000000000000000, -0.000000000000000000 ) ) ;
#2210 = VECTOR ( 'NONE', #20023, 1000.000000000000000 ) ;
#2211 = ORIENTED_EDGE ( 'NONE', *, *, #20541, .T. ) ;
#2212 = VERTEX_POINT ( 'NONE', #17883 ) ;
#2213 = CARTESIAN_POINT ( 'NONE',  ( 7.516414041016176384, 19.83100852729402064, -1.255802337575999905 ) ) ;
#2214 = DIRECTION ( 'NONE',  ( -0.000000000000000000, -1.000000000000000000, 0.000000000000000000 ) ) ;
#2215 = CARTESIAN_POINT ( 'NONE',  ( 12.12180015326468485, 10.40596899240396311, 1.263324329328538109 ) ) ;
#2216 = VERTEX_POINT ( 'NONE', #2729 ) ;
#2217 = VERTEX_POINT ( 'NONE', #21294 ) ;
#2218 = CIRCLE ( 'NONE', #18453, 3.970019999999998550 ) ;
#2219 = DIRECTION ( 'NONE',  ( 0.000000000000000000, 1.000000000000000000, 0.000000000000000000 ) ) ;
#2220 = CARTESIAN_POINT ( 'NONE',  ( 8.113089735847959005, 10.84140768076111172, 1.524413057128902294 ) ) ;
#2221 = CIRCLE ( 'NONE', #3289, 0.3962399999999997591 ) ;
#2222 = CARTESIAN_POINT ( 'NONE',  ( 5.651855977748085458, 20.83490078207852392, 3.725216732626875693 ) ) ;
#2223 = FACE_OUTER_BOUND ( 'NONE', #2461, .T. ) ;
#2224 = ADVANCED_FACE ( 'NONE', ( #6153 ), #15861, .T. ) ;
#2225 = CARTESIAN_POINT ( 'NONE',  ( 5.917177850220659785, 12.44752302178212133, 0.6815623641613539618 ) ) ;
#2226 = CARTESIAN_POINT ( 'NONE',  ( 1.954387715434429795, 8.736780638212259475, 10.71562499999999929 ) ) ;
#2227 = VECTOR ( 'NONE', #21862, 1000.000000000000000 ) ;
#2228 = ADVANCED_FACE ( 'NONE', ( #5563 ), #3924, .T. ) ;
#2229 = CARTESIAN_POINT ( 'NONE',  ( 10.07533004185552272, 21.75488213915048163, 3.488364678943705943 ) ) ;
#2230 = CARTESIAN_POINT ( 'NONE',  ( 17.85969298310271114, 32.52628750000000224, 1.318856445756055873 ) ) ;
#2231 = CARTESIAN_POINT ( 'NONE',  ( 1.840183766054111159, 21.28931287393832150, 5.000021689193579810 ) ) ;
#2232 = CARTESIAN_POINT ( 'NONE',  ( 0.8789596239274352074, 19.99575406279286582, 7.958759135206050495 ) ) ;
#2233 = VECTOR ( 'NONE', #21115, 1000.000000000000000 ) ;
#2234 = AXIS2_PLACEMENT_3D ( 'NONE', #14022, #2275, #17644 ) ;
#2235 = CARTESIAN_POINT ( 'NONE',  ( 6.650780717571844747, 11.71035962591412272, 4.098950421500386909 ) ) ;
#2236 = CYLINDRICAL_SURFACE ( 'NONE', #1428, 0.7950200000000000600 ) ;
#2237 = CARTESIAN_POINT ( 'NONE',  ( -2.256261688646920227, 9.129395000000000593, -0.3933872460174320240 ) ) ;
#2238 = CARTESIAN_POINT ( 'NONE',  ( 14.08131258074581105, 1.962522422995664151, -16.02478678334940554 ) ) ;
#2239 = EDGE_CURVE ( 'NONE', #20753, #11503, #4571, .T. ) ;
#2240 = EDGE_CURVE ( 'NONE', #20891, #13567, #9292, .T. ) ;
#2241 = CARTESIAN_POINT ( 'NONE',  ( 6.396056618077795797, 11.71523274630726164, 2.847703469759983008 ) ) ;
#2242 = CARTESIAN_POINT ( 'NONE',  ( 10.84114159136082556, 11.15340055693774346, 4.434419607208564429 ) ) ;
#2243 = ORIENTED_EDGE ( 'NONE', *, *, #1751, .F. ) ;
#2244 = VECTOR ( 'NONE', #14358, 1000.000000000000227 ) ;
#2245 = FACE_OUTER_BOUND ( 'NONE', #13627, .T. ) ;
#2246 = CARTESIAN_POINT ( 'NONE',  ( 11.17813456493683688, 16.31200234120390391, -3.589686200531655658 ) ) ;
#2247 = DIRECTION ( 'NONE',  ( 0.9579671649362032637, 0.000000000000000000, -0.2868778675745010664 ) ) ;
#2248 = VERTEX_POINT ( 'NONE', #14984 ) ;
#2249 = APPLICATION_PROTOCOL_DEFINITION ( 'draft international standard', 'automotive_design', 1998, #6216 ) ;
#2250 = CARTESIAN_POINT ( 'NONE',  ( 1.291462649553455133, -1.594802499999998124, -20.78637864442906746 ) ) ;
#2251 = CIRCLE ( 'NONE', #18482, 0.5080000000000005622 ) ;
#2252 = CYLINDRICAL_SURFACE ( 'NONE', #1570, 1.785937500000001510 ) ;
#2253 = CARTESIAN_POINT ( 'NONE',  ( 20.51985202635208694, -6.011610439988455568, -14.03095391611717346 ) ) ;
#2254 = ORIENTED_EDGE ( 'NONE', *, *, #6519, .T. ) ;
#2255 = CARTESIAN_POINT ( 'NONE',  ( 12.23442992331478330, 20.89186537925146325, -1.172561438593525462 ) ) ;
#2256 = CARTESIAN_POINT ( 'NONE',  ( 4.218669509945208951, 20.25152453169299349, 5.586594807314953393 ) ) ;
#2257 = AXIS2_PLACEMENT_3D ( 'NONE', #14167, #7396, #12497 ) ;
#2258 = CARTESIAN_POINT ( 'NONE',  ( 5.589282794631477813, 15.56565457311297251, -1.430601909125969406 ) ) ;
#2259 = CARTESIAN_POINT ( 'NONE',  ( 42.35466991749225940, 0.000000000000000000, -17.94967221382040279 ) ) ;
#2260 = CARTESIAN_POINT ( 'NONE',  ( 19.84534036711146143, -1.573540299197002224, -15.46898262837090243 ) ) ;
#2261 = CARTESIAN_POINT ( 'NONE',  ( 16.91309518241949661, 0.9412279162453636161, -15.17502221664437911 ) ) ;
#2262 = EDGE_CURVE ( 'NONE', #2328, #20984, #4718, .T. ) ;
#2263 = CARTESIAN_POINT ( 'NONE',  ( 0.7843704457339527591, 25.39269750000000059, -23.55949434567611078 ) ) ;
#2264 = ORIENTED_EDGE ( 'NONE', *, *, #18406, .F. ) ;
#2265 = CARTESIAN_POINT ( 'NONE',  ( 6.056291209943008624, 11.11068921130002174, 1.344815542909726380 ) ) ;
#2266 = AXIS2_PLACEMENT_3D ( 'NONE', #19432, #11373, #9591 ) ;
#2267 = DIRECTION ( 'NONE',  ( 0.000000000000000000, 1.000000000000000000, 0.000000000000000000 ) ) ;
#2268 = ORIENTED_EDGE ( 'NONE', *, *, #13671, .F. ) ;
#2269 = CARTESIAN_POINT ( 'NONE',  ( 9.524025606199806759, 12.69250285052379645, -1.295200290336259608 ) ) ;
#2270 = CARTESIAN_POINT ( 'NONE',  ( -14.17069798364451927, -1.594802499999999013, -10.28222191653059170 ) ) ;
#2271 = DIRECTION ( 'NONE',  ( -0.9685006480810794960, 0.000000000000000000, -0.2490110332224836354 ) ) ;
#2273 = DIRECTION ( 'NONE',  ( 0.000000000000000000, 0.000000000000000000, -1.000000000000000000 ) ) ;
#2272 = CARTESIAN_POINT ( 'NONE',  ( 0.7719978298209800860, 18.72099911278871787, 8.787022842826415214 ) ) ;
#2274 = ORIENTED_EDGE ( 'NONE', *, *, #4323, .F. ) ;
#2275 = DIRECTION ( 'NONE',  ( 0.000000000000000000, 0.000000000000000000, 1.000000000000000000 ) ) ;
#2276 = VECTOR ( 'NONE', #11207, 1000.000000000000000 ) ;
#2277 = FACE_OUTER_BOUND ( 'NONE', #16147, .T. ) ;
#2278 = EDGE_LOOP ( 'NONE', ( #17666, #4526, #8474, #2014, #7296, #13122 ) ) ;
#2279 = DIRECTION ( 'NONE',  ( 0.05085730733808142834, 0.000000000000000000, -0.9987059298363657467 ) ) ;
#2280 = CARTESIAN_POINT ( 'NONE',  ( 14.37256150657012199, 1.100706393900077407, -15.89788116173771648 ) ) ;
#2281 = ORIENTED_EDGE ( 'NONE', *, *, #19742, .F. ) ;
#2282 = CARTESIAN_POINT ( 'NONE',  ( 52.19854938732527216, 38.88803500000000213, -17.58284632693144189 ) ) ;
#2283 = CARTESIAN_POINT ( 'NONE',  ( 2.092738645373398043, 17.72593790894276822, 0.2727642672195841334 ) ) ;
#2284 = VECTOR ( 'NONE', #16090, 1000.000000000000000 ) ;
#2285 = CARTESIAN_POINT ( 'NONE',  ( 9.124037948774077478, 15.28165795756530265, -3.667571731158457471 ) ) ;
#2286 = FACE_OUTER_BOUND ( 'NONE', #4386, .T. ) ;
#2287 = AXIS2_PLACEMENT_3D ( 'NONE', #20417, #1754, #4969 ) ;
#2288 = EDGE_CURVE ( 'NONE', #1054, #20069, #12884, .T. ) ;
#2289 = CARTESIAN_POINT ( 'NONE',  ( 2.492193568723835462, -69.63187750000000165, -24.56873394466936134 ) ) ;
#2290 = ORIENTED_EDGE ( 'NONE', *, *, #4296, .T. ) ;
#2291 = CARTESIAN_POINT ( 'NONE',  ( 1.532169971477637782, 34.03012968715594866, -20.71839214105750315 ) ) ;
#2292 = CARTESIAN_POINT ( 'NONE',  ( 20.36270583931112910, -6.627754957419618620, -15.18422494847827586 ) ) ;
#2294 = CARTESIAN_POINT ( 'NONE',  ( -1.880134707694870011, 20.24316500000000119, 7.779750394130780400 ) ) ;
#2293 = FACE_OUTER_BOUND ( 'NONE', #15401, .T. ) ;
#2295 = ORIENTED_EDGE ( 'NONE', *, *, #2372, .F. ) ;
#2296 = ORIENTED_EDGE ( 'NONE', *, *, #6544, .F. ) ;
#2297 = CARTESIAN_POINT ( 'NONE',  ( 3.021518493146395201, 19.78048590522542227, 7.993777974749627369 ) ) ;
#2298 = VERTEX_POINT ( 'NONE', #14868 ) ;
#2300 = CARTESIAN_POINT ( 'NONE',  ( 11.30427477552373894, 0.1855068411375157544, -16.71599931165275521 ) ) ;
#2299 = CARTESIAN_POINT ( 'NONE',  ( 5.205980611946986691, 11.94362822924763634, 6.505740943259474385 ) ) ;
#2301 = ORIENTED_EDGE ( 'NONE', *, *, #9369, .F. ) ;
#2302 = VERTEX_POINT ( 'NONE', #21585 ) ;
#2303 = AXIS2_PLACEMENT_3D ( 'NONE', #6826, #18541, #18638 ) ;
#2304 = CARTESIAN_POINT ( 'NONE',  ( 1.345719439226387371, 13.41272998646361714, 7.668264603079712138 ) ) ;
#2305 = ORIENTED_EDGE ( 'NONE', *, *, #3869, .F. ) ;
#2306 = CARTESIAN_POINT ( 'NONE',  ( 12.13621795668766445, 36.51313500000000545, 4.225309685850866082 ) ) ;
#2307 = CARTESIAN_POINT ( 'NONE',  ( -0.02450470937351344886, 0.004533752046478279826, 8.892108737872939983 ) ) ;
#2308 = DIRECTION ( 'NONE',  ( -0.9685006480810790519, 0.000000000000000000, -0.2490110332224857170 ) ) ;
#2309 = CARTESIAN_POINT ( 'NONE',  ( 14.43917063414567536, 39.28268749999999443, 2.343183994106907697 ) ) ;
#2310 = FACE_OUTER_BOUND ( 'NONE', #21323, .T. ) ;
#2311 = CARTESIAN_POINT ( 'NONE',  ( 3.025083360574306379, 19.58333031856296103, 8.033243523162543198 ) ) ;
#2312 = EDGE_CURVE ( 'NONE', #10134, #7286, #8239, .T. ) ;
#2313 = CARTESIAN_POINT ( 'NONE',  ( 53.45144661199496028, 38.88803500000000213, -15.40991637425222827 ) ) ;
#2314 = EDGE_LOOP ( 'NONE', ( #18332, #4923, #10343, #5168 ) ) ;
#2315 = CARTESIAN_POINT ( 'NONE',  ( 4.226748096773134122, 12.75273057655540043, 0.7412141520461309474 ) ) ;
#2316 = CARTESIAN_POINT ( 'NONE',  ( 17.22522857595987844, -1.983739999999999393, -15.04442098945225403 ) ) ;
#2317 = CARTESIAN_POINT ( 'NONE',  ( 13.37542130762736647, 22.16307796594318802, 1.955246718568947273 ) ) ;
#2318 = PLANE ( 'NONE',  #21251 ) ;
#2319 = TOROIDAL_SURFACE ( 'NONE', #21731, 3.174999999999999822, 0.5953125000000000222 ) ;
#2320 = CYLINDRICAL_SURFACE ( 'NONE', #2800, 30.16250000000000142 ) ;
#2321 = ORIENTED_EDGE ( 'NONE', *, *, #10762, .F. ) ;
#2322 = ORIENTED_EDGE ( 'NONE', *, *, #1035, .F. ) ;
#2323 = CARTESIAN_POINT ( 'NONE',  ( 8.698080803895434698, 18.39925938975357056, 7.424547285105621341 ) ) ;
#2325 = DIRECTION ( 'NONE',  ( 0.000000000000000000, 1.000000000000000000, 0.000000000000000000 ) ) ;
#2324 = CARTESIAN_POINT ( 'NONE',  ( 1.854799496439154316, 16.26393749999999727, 3.211081754263136911 ) ) ;
#2326 = CARTESIAN_POINT ( 'NONE',  ( 12.02571325582669282, 10.42810541502117161, 0.8657527866613862200 ) ) ;
#2327 = EDGE_LOOP ( 'NONE', ( #10719, #6356, #8378, #18238 ) ) ;
#2328 = VERTEX_POINT ( 'NONE', #9649 ) ;
#2329 = DIRECTION ( 'NONE',  ( -0.9579671649362030417, 0.000000000000000000, 0.2868778675745017326 ) ) ;
#2330 = CARTESIAN_POINT ( 'NONE',  ( 7.711757841094235566, 11.51867810285771121, -0.1922238782181159011 ) ) ;
#2331 = CARTESIAN_POINT ( 'NONE',  ( 47.80475250345343596, -7.547610000000002373, -11.91473563638196786 ) ) ;
#2332 = LINE ( 'NONE', #5862, #1679 ) ;
#2333 = CARTESIAN_POINT ( 'NONE',  ( 5.786084785701969935, 17.74437171614160391, -1.199539018687937331 ) ) ;
#2334 = CARTESIAN_POINT ( 'NONE',  ( 7.130351268715567237, 12.94937010301612723, 6.204865410933570580 ) ) ;
#2335 = CYLINDRICAL_SURFACE ( 'NONE', #15678, 1.190625000000000488 ) ;
#2336 = EDGE_CURVE ( 'NONE', #15924, #15199, #7891, .T. ) ;
#2337 = CARTESIAN_POINT ( 'NONE',  ( 6.344892231242216241, 11.19290776549860134, 1.289291468351646763 ) ) ;
#2338 = CARTESIAN_POINT ( 'NONE',  ( 4.898461982228181633, 12.16261474950084498, 5.232768426419909247 ) ) ;
#2339 = CARTESIAN_POINT ( 'NONE',  ( 32.55306802826559220, 0.000000000000000000, -17.37731658638881527 ) ) ;
#2340 = DIRECTION ( 'NONE',  ( 0.9876802608827760510, 0.000000000000000000, -0.1564854698127960131 ) ) ;
#2341 = CARTESIAN_POINT ( 'NONE',  ( 6.266996954026719635, 21.18238311700324417, 5.546799428808435017 ) ) ;
#2342 = CARTESIAN_POINT ( 'NONE',  ( 1.266019147034259884, 18.88490084365312782, 8.903593704730354830 ) ) ;
#2343 = ADVANCED_FACE ( 'NONE', ( #7989 ), #18060, .T. ) ;
#2344 = ADVANCED_FACE ( 'NONE', ( #13865 ), #677, .F. ) ;
#2345 = EDGE_CURVE ( 'NONE', #13041, #20031, #19352, .T. ) ;
#2346 = CARTESIAN_POINT ( 'NONE',  ( 65.51436440461340283, 1.984375000000000000, -12.87863775929475985 ) ) ;
#2347 = CARTESIAN_POINT ( 'NONE',  ( 1.828908678823709666, 20.48283743933590273, 4.930034699729209713 ) ) ;
#2348 = DIRECTION ( 'NONE',  ( 0.000000000000000000, 1.000000000000000000, 0.000000000000000000 ) ) ;
#2349 = DIRECTION ( 'NONE',  ( -0.000000000000000000, -1.000000000000000000, 0.000000000000000000 ) ) ;
#2350 = CARTESIAN_POINT ( 'NONE',  ( 12.80562560408363915, 1.259733001188390489, -16.40790845565960510 ) ) ;
#2351 = DIRECTION ( 'NONE',  ( -0.1060008583745199739, 0.000000000000000000, -0.9943660382494290406 ) ) ;
#2352 = CARTESIAN_POINT ( 'NONE',  ( 9.688677822838410947, 11.12736925383730124, -0.4069968778330486092 ) ) ;
#2353 = ORIENTED_EDGE ( 'NONE', *, *, #5626, .T. ) ;
#2354 = CARTESIAN_POINT ( 'NONE',  ( 49.13030338002142372, -9.531985000000000596, -2.154981381712871791 ) ) ;
#2355 = CARTESIAN_POINT ( 'NONE',  ( 11.47251706867474041, 12.23848474711970802, -1.592967478809933723 ) ) ;
#2356 = CARTESIAN_POINT ( 'NONE',  ( 5.656534285913039639, 12.27047075047317115, -0.3509529794051957086 ) ) ;
#2357 = LINE ( 'NONE', #19271, #10550 ) ;
#2358 = CARTESIAN_POINT ( 'NONE',  ( 0.3202639567549845911, 18.57485916386803382, 1.339964575302207805 ) ) ;
#2359 = ORIENTED_EDGE ( 'NONE', *, *, #4471, .T. ) ;
#2360 = CONTEXT_DEPENDENT_SHAPE_REPRESENTATION ( #1280, #17108 ) ;
#2361 = FACE_OUTER_BOUND ( 'NONE', #13362, .T. ) ;
#2362 = CARTESIAN_POINT ( 'NONE',  ( 6.060393788137320215, 20.48930581516298233, 4.878321978022181149 ) ) ;
#2363 = VECTOR ( 'NONE', #21213, 1000.000000000000000 ) ;
#2364 = CARTESIAN_POINT ( 'NONE',  ( 9.262381024405307528, 30.63641399982339308, -21.59935919086856515 ) ) ;
#2365 = EDGE_CURVE ( 'NONE', #1425, #17778, #19192, .T. ) ;
#2366 = CARTESIAN_POINT ( 'NONE',  ( 11.33696792159741662, 0.1808088057320689224, -16.81606727879834651 ) ) ;
#2367 = ORIENTED_EDGE ( 'NONE', *, *, #17924, .F. ) ;
#2368 = CARTESIAN_POINT ( 'NONE',  ( 6.496396028925151889, 20.04364414270774120, 0.1831189632268445389 ) ) ;
#2369 = CARTESIAN_POINT ( 'NONE',  ( 7.588986978588807553, 13.14768317755540039, -1.065587204641165409 ) ) ;
#2370 = DIRECTION ( 'NONE',  ( 0.000000000000000000, 1.000000000000000000, 0.000000000000000000 ) ) ;
#2371 = CARTESIAN_POINT ( 'NONE',  ( 12.81298227213678942, 22.28511555871962102, 0.3971908496776146991 ) ) ;
#2372 = EDGE_CURVE ( 'NONE', #1209, #19005, #10519, .T. ) ;
#2373 = CARTESIAN_POINT ( 'NONE',  ( 61.04701390398659555, 0.000000000000000000, -15.15157976445104993 ) ) ;
#2374 = CARTESIAN_POINT ( 'NONE',  ( 12.56940319628321490, -0.6962962921986948217, -16.53391742796571151 ) ) ;
#2375 = LINE ( 'NONE', #20819, #10264 ) ;
#2376 = VECTOR ( 'NONE', #10947, 1000.000000000000000 ) ;
#2377 = ORIENTED_EDGE ( 'NONE', *, *, #3048, .F. ) ;
#2378 = CARTESIAN_POINT ( 'NONE',  ( 11.16649006228652041, 16.55586016349425194, 6.818406148130505606 ) ) ;
#2379 = CARTESIAN_POINT ( 'NONE',  ( 6.794028650656957602, 11.05210752777782091, 4.465890901017215420 ) ) ;
#2380 = CARTESIAN_POINT ( 'NONE',  ( 1.268730000000000135, 23.41816500000000190, 8.609509071587499562 ) ) ;
#2381 = EDGE_LOOP ( 'NONE', ( #6945, #15252, #13580, #3398 ) ) ;
#2382 = CARTESIAN_POINT ( 'NONE',  ( 9.926485704785847020, 11.59865289762421270, 0.5377904742533208271 ) ) ;
#2383 = LINE ( 'NONE', #15450, #8838 ) ;
#2384 = CARTESIAN_POINT ( 'NONE',  ( 0.02376778487644688048, 20.19881069607145108, 5.688190597157388950 ) ) ;
#2386 = DIRECTION ( 'NONE',  ( 1.000000000000000000, 0.000000000000000000, 0.000000000000000000 ) ) ;
#2385 = CARTESIAN_POINT ( 'NONE',  ( 0.9792782680767874171, 12.85015660565266060, 7.901049221702420411 ) ) ;
#2387 = ORIENTED_EDGE ( 'NONE', *, *, #13897, .T. ) ;
#2388 = CARTESIAN_POINT ( 'NONE',  ( 7.520682447844541763, 16.20627867842422631, 8.395911810959326260 ) ) ;
#2389 = LINE ( 'NONE', #6846, #11320 ) ;
#2390 = DIRECTION ( 'NONE',  ( 0.5734623443633278805, 0.8192319205190407017, 0.000000000000000000 ) ) ;
#2391 = ORIENTED_EDGE ( 'NONE', *, *, #11011, .F. ) ;
#2392 = CARTESIAN_POINT ( 'NONE',  ( 19.33923522922928839, 0.3748380676697945502, -15.04264288269788885 ) ) ;
#2393 = EDGE_CURVE ( 'NONE', #21254, #13041, #13982, .T. ) ;
#2394 = CARTESIAN_POINT ( 'NONE',  ( 0.02905096893341448799, 15.40301703741441663, 0.9139028180173993654 ) ) ;
#2395 = EDGE_CURVE ( 'NONE', #3338, #7171, #493, .T. ) ;
#2396 = VECTOR ( 'NONE', #17884, 1000.000000000000000 ) ;
#2397 = CARTESIAN_POINT ( 'NONE',  ( 14.55664670201521638, -7.269926523219644388, -16.33216676728327599 ) ) ;
#2398 = ORIENTED_EDGE ( 'NONE', *, *, #18799, .T. ) ;
#2399 = CARTESIAN_POINT ( 'NONE',  ( 53.25483508941461963, 0.000000000000000000, -5.879799058943532941 ) ) ;
#2400 = LINE ( 'NONE', #4392, #3205 ) ;
#2401 = CARTESIAN_POINT ( 'NONE',  ( 12.56778430086266063, 10.42448595387692301, 2.703119026783505685 ) ) ;
#2402 = DIRECTION ( 'NONE',  ( 1.000000000000000000, 0.000000000000000000, 0.000000000000000000 ) ) ;
#2403 = CARTESIAN_POINT ( 'NONE',  ( 38.96521490655496223, -7.547609999999999708, -3.938433986281342225 ) ) ;
#2404 = ORIENTED_EDGE ( 'NONE', *, *, #11133, .T. ) ;
#2405 = DIRECTION ( 'NONE',  ( 0.6702301885068628895, 0.000000000000000000, 0.7421532822901579785 ) ) ;
#2407 = DIRECTION ( 'NONE',  ( -0.9964481331860212121, 0.000000000000000000, 0.08420877549337300871 ) ) ;
#2406 = CARTESIAN_POINT ( 'NONE',  ( 13.67756757867809725, 38.48766750000000059, 2.571257636385987144 ) ) ;
#2408 = ORIENTED_EDGE ( 'NONE', *, *, #389, .F. ) ;
#2409 = VERTEX_POINT ( 'NONE', #19252 ) ;
#2410 = VECTOR ( 'NONE', #7152, 1000.000000000000114 ) ;
#2412 = CARTESIAN_POINT ( 'NONE',  ( -1.848761088705630051, 23.41816500000000190, 7.884515871828260636 ) ) ;
#2411 = CARTESIAN_POINT ( 'NONE',  ( 1.699527425015976645, 13.92038700339129242, 9.102769882603862328 ) ) ;
#2413 = ORIENTED_EDGE ( 'NONE', *, *, #12523, .F. ) ;
#2414 = CARTESIAN_POINT ( 'NONE',  ( 5.247544535690431111, 12.08598944411757792, 6.695756513832588297 ) ) ;
#2415 = ORIENTED_EDGE ( 'NONE', *, *, #7631, .T. ) ;
#2416 = ORIENTED_EDGE ( 'NONE', *, *, #15750, .T. ) ;
#2417 = CARTESIAN_POINT ( 'NONE',  ( 1.327405647319859439, 13.31436210545662213, 7.568774271523563080 ) ) ;
#2418 = ADVANCED_FACE ( 'NONE', ( #7320 ), #12295, .F. ) ;
#2419 = ORIENTED_EDGE ( 'NONE', *, *, #1951, .F. ) ;
#2420 = CARTESIAN_POINT ( 'NONE',  ( 3.296278299113588606, 13.37815361419331062, 7.298396853533315465 ) ) ;
#2421 = VECTOR ( 'NONE', #18715, 1000.000000000000114 ) ;
#2422 = CARTESIAN_POINT ( 'NONE',  ( -47.86112874365709047, -10.87373999999999974, -23.29368419115692035 ) ) ;
#2423 = CARTESIAN_POINT ( 'NONE',  ( 31.02798609601340729, 0.000000000000000000, -5.485920235548950252 ) ) ;
#2424 = CARTESIAN_POINT ( 'NONE',  ( 61.56621290189396944, -1.983739999999999837, -0.7977859469341201937 ) ) ;
#2425 = PRODUCT_DEFINITION_SHAPE ( 'NONE', 'NONE',  #3715 ) ;
#2426 = CARTESIAN_POINT ( 'NONE',  ( 55.27198911326564001, 32.54502000000000095, 2.462719476673013830 ) ) ;
#2427 = CARTESIAN_POINT ( 'NONE',  ( 1.164373365471405464, 20.93742321894627167, 3.100345057572924556 ) ) ;
#2428 = DIRECTION ( 'NONE',  ( 0.8741107132214044340, 0.000000000000000000, 0.4857267349359799535 ) ) ;
#2429 = VERTEX_POINT ( 'NONE', #5772 ) ;
#2430 = CARTESIAN_POINT ( 'NONE',  ( 6.264679519144333852, 12.20187417505221994, 0.8393449708032283407 ) ) ;
#2431 = CARTESIAN_POINT ( 'NONE',  ( 11.11706420665069217, -4.717387944073672124, -16.40916909168538496 ) ) ;
#2432 = DIRECTION ( 'NONE',  ( -0.5087559856598092844, 0.000000000000000000, -0.8609107660235849613 ) ) ;
#2433 = PLANE ( 'NONE',  #789 ) ;
#2434 = VERTEX_POINT ( 'NONE', #14082 ) ;
#2435 = ORIENTED_EDGE ( 'NONE', *, *, #21472, .F. ) ;
#2436 = CARTESIAN_POINT ( 'NONE',  ( 8.937652522793825938, 16.60610825764645071, 7.830010146707459207 ) ) ;
#2438 = DIRECTION ( 'NONE',  ( 0.5087559856598092844, 0.000000000000000000, 0.8609107660235849613 ) ) ;
#2437 = DIRECTION ( 'NONE',  ( 0.000000000000000000, -1.000000000000000000, -0.000000000000000000 ) ) ;
#2439 = CARTESIAN_POINT ( 'NONE',  ( 12.46883308523603695, 10.55182128074574166, 2.701636765429729969 ) ) ;
#2440 = ORIENTED_EDGE ( 'NONE', *, *, #8438, .T. ) ;
#2441 = ORIENTED_EDGE ( 'NONE', *, *, #5568, .T. ) ;
#2442 = LINE ( 'NONE', #10945, #6725 ) ;
#2443 = AXIS2_PLACEMENT_3D ( 'NONE', #4092, #7521, #10832 ) ;
#2444 = CARTESIAN_POINT ( 'NONE',  ( 7.810601781778314212, 11.28094437888862167, 0.2371453506886788687 ) ) ;
#2445 = CARTESIAN_POINT ( 'NONE',  ( 2.224701653548029512, 12.53189561649392125, 2.144358178734434350 ) ) ;
#2446 = CYLINDRICAL_SURFACE ( 'NONE', #1340, 0.5079999999999996740 ) ;
#2447 = CARTESIAN_POINT ( 'NONE',  ( 8.802231832380332577, 18.96461393410900342, 6.449481405740358220 ) ) ;
#2448 = CARTESIAN_POINT ( 'NONE',  ( 7.323594443806002552, 14.97599272452439934, 7.432113103085323580 ) ) ;
#2449 = EDGE_CURVE ( 'NONE', #1010, #10254, #2856, .T. ) ;
#2450 = CARTESIAN_POINT ( 'NONE',  ( 59.89111109153450485, 29.95901653600000003, -22.14529389979288965 ) ) ;
#2451 = VECTOR ( 'NONE', #11304, 1000.000000000000114 ) ;
#2452 = DIRECTION ( 'NONE',  ( -0.9987059298363656357, 0.000000000000000000, -0.05085730733808393328 ) ) ;
#2453 = CARTESIAN_POINT ( 'NONE',  ( 5.655654580052440039, 15.45793682862229801, -2.195876644601166383 ) ) ;
#2454 = CARTESIAN_POINT ( 'NONE',  ( 0.9710684863527534461, 19.78858245918292980, 8.191681233637670090 ) ) ;
#2455 = CIRCLE ( 'NONE', #13065, 30.16249999999998366 ) ;
#2456 = PLANE ( 'NONE',  #1174 ) ;
#2457 = CARTESIAN_POINT ( 'NONE',  ( 1.479868076741676086, 15.70115217790233508, 8.893450642701147046 ) ) ;
#2458 = CARTESIAN_POINT ( 'NONE',  ( 30.47347900023190803, 32.54502000000000095, -8.148724574017967015 ) ) ;
#2459 = DIRECTION ( 'NONE',  ( 0.2490110332224836354, 0.000000000000000000, -0.9685006480810794960 ) ) ;
#2460 = CARTESIAN_POINT ( 'NONE',  ( 20.82734621676318199, -1.850212124675815195, -13.95953525842948828 ) ) ;
#2461 = EDGE_LOOP ( 'NONE', ( #884, #4206, #14313, #10118, #4181, #10108, #18999, #16892, #15929, #1766, #8567, #19717, #16820, #19420, #14827, #10153, #7652, #7601, #20757, #17660, #1472, #1047, #8293, #7481, #4823, #18978, #17213, #16162 ) ) ;
#2462 = CARTESIAN_POINT ( 'NONE',  ( 59.80894853325292360, -6.356984999999999886, -16.70545285374888778 ) ) ;
#2463 = AXIS2_PLACEMENT_3D ( 'NONE', #9443, #11327, #18078 ) ;
#2464 = CARTESIAN_POINT ( 'NONE',  ( 10.32679327456467711, 10.57999906717443217, 2.270008812520685204 ) ) ;
#2465 = EDGE_LOOP ( 'NONE', ( #13573, #15352 ) ) ;
#2466 = EDGE_CURVE ( 'NONE', #21748, #1981, #7554, .T. ) ;
#2467 = CARTESIAN_POINT ( 'NONE',  ( -15.97216256926745714, -95.96551800000000298, -9.259783438096400587 ) ) ;
#2468 = CARTESIAN_POINT ( 'NONE',  ( 5.951137870369475280, 11.39017030426189159, 0.9629264744454320013 ) ) ;
#2469 = CARTESIAN_POINT ( 'NONE',  ( 30.41963056417667488, 32.54502000000000095, -8.653862521447852174 ) ) ;
#2470 = EDGE_LOOP ( 'NONE', ( #5241, #5173 ) ) ;
#2471 = SURFACE_STYLE_USAGE ( .BOTH. , #15984 ) ;
#2472 = EDGE_CURVE ( 'NONE', #9581, #2549, #6850, .T. ) ;
#2473 = ADVANCED_FACE ( 'NONE', ( #7749, #3101, #8066 ), #14631, .F. ) ;
#2474 = CARTESIAN_POINT ( 'NONE',  ( 20.76310168089343478, 34.52875999999999834, -11.26763008640078212 ) ) ;
#2475 = CARTESIAN_POINT ( 'NONE',  ( 17.53455994494808223, -8.551185372775542248, -15.70422118946672363 ) ) ;
#2476 = ORIENTED_EDGE ( 'NONE', *, *, #19653, .F. ) ;
#2477 = CARTESIAN_POINT ( 'NONE',  ( 8.288275297767960126, 11.49260726995666104, 1.826824681916124016 ) ) ;
#2478 = VECTOR ( 'NONE', #10363, 1000.000000000000000 ) ;
#2479 = CIRCLE ( 'NONE', #14857, 30.16249999999999432 ) ;
#2480 = CARTESIAN_POINT ( 'NONE',  ( 11.17045701329781870, 16.27078922038444375, -3.703851085504920704 ) ) ;
#2481 = DIRECTION ( 'NONE',  ( 0.000000000000000000, -1.000000000000000000, -0.000000000000000000 ) ) ;
#2482 = CARTESIAN_POINT ( 'NONE',  ( 5.232332039340263030, 18.73163945740397196, 8.232832001541300571 ) ) ;
#2483 = DIRECTION ( 'NONE',  ( 0.000000000000000000, -1.000000000000000000, 0.000000000000000000 ) ) ;
#2484 = AXIS2_PLACEMENT_3D ( 'NONE', #7530, #14395, #14186 ) ;
#2485 = ORIENTED_EDGE ( 'NONE', *, *, #1311, .F. ) ;
#2486 = CARTESIAN_POINT ( 'NONE',  ( 13.00775088886534014, 18.81300736124048001, 6.802859426759906292 ) ) ;
#2487 = EDGE_CURVE ( 'NONE', #5219, #13475, #12963, .T. ) ;
#2488 = CARTESIAN_POINT ( 'NONE',  ( 52.19854938732527216, 39.04666396067986511, -17.58284632693144189 ) ) ;
#2489 = ORIENTED_EDGE ( 'NONE', *, *, #16116, .F. ) ;
#2490 = CARTESIAN_POINT ( 'NONE',  ( 9.718623483178818745, 12.00923416725010107, -0.3876423491285933554 ) ) ;
#2491 = DIRECTION ( 'NONE',  ( 0.2490110332224846346, 0.000000000000000000, -0.9685006480810792739 ) ) ;
#2492 = CARTESIAN_POINT ( 'NONE',  ( 1.218747862079375022, 17.86133278564378557, 8.560453536580162393 ) ) ;
#2494 = FACE_OUTER_BOUND ( 'NONE', #2970, .T. ) ;
#2493 = CARTESIAN_POINT ( 'NONE',  ( 3.023071641832506984, 21.04679274153226132, 3.678863645485955569 ) ) ;
#2495 = VERTEX_POINT ( 'NONE', #9826 ) ;
#2496 = CARTESIAN_POINT ( 'NONE',  ( -17.46249999999999858, 32.54247999999999763, 0.000000000000000000 ) ) ;
#2497 = CARTESIAN_POINT ( 'NONE',  ( 39.79827138724637337, -6.045821519594339222, -3.121440830586406090 ) ) ;
#2498 = VERTEX_POINT ( 'NONE', #19892 ) ;
#2499 = ADVANCED_FACE ( 'NONE', ( #7643 ), #21337, .F. ) ;
#2500 = CARTESIAN_POINT ( 'NONE',  ( 19.39574039404867278, 0.4330848887872487118, -14.99545623812619866 ) ) ;
#2501 = VECTOR ( 'NONE', #21012, 1000.000000000000000 ) ;
#2502 = CARTESIAN_POINT ( 'NONE',  ( 19.50328736735570345, -0.8676315445611676447, -15.54195256409067483 ) ) ;
#2503 = ORIENTED_EDGE ( 'NONE', *, *, #5945, .T. ) ;
#2504 = DIRECTION ( 'NONE',  ( 0.000000000000000000, 1.000000000000000000, 0.000000000000000000 ) ) ;
#2505 = CARTESIAN_POINT ( 'NONE',  ( 1.899735969233180333, 16.00403838164227110, 0.07924708280844300345 ) ) ;
#2506 = CARTESIAN_POINT ( 'NONE',  ( 13.51152013350133352, 14.65422691944639766, 7.038129281359358558 ) ) ;
#2507 = DIRECTION ( 'NONE',  ( 0.000000000000000000, 1.000000000000000000, 0.000000000000000000 ) ) ;
#2508 = DIRECTION ( 'NONE',  ( 0.000000000000000000, 1.000000000000000000, 0.000000000000000000 ) ) ;
#2509 = VERTEX_POINT ( 'NONE', #21230 ) ;
#2510 = DIRECTION ( 'NONE',  ( 0.9685006480810790519, 0.000000000000000000, 0.2490110332224857170 ) ) ;
#2511 = EDGE_CURVE ( 'NONE', #7874, #13814, #4187, .T. ) ;
#2513 = CARTESIAN_POINT ( 'NONE',  ( 2.915917464538113180, 34.52875999999999834, -18.72348548116188027 ) ) ;
#2512 = CARTESIAN_POINT ( 'NONE',  ( 31.75000000000000000, 32.54502000000000095, -4.317999999999999616 ) ) ;
#2514 = STYLED_ITEM ( 'NONE', ( #13999 ), #6428 ) ;
#2515 = ORIENTED_EDGE ( 'NONE', *, *, #3919, .F. ) ;
#2516 = EDGE_CURVE ( 'NONE', #20607, #8815, #16278, .T. ) ;
#2517 = ORIENTED_EDGE ( 'NONE', *, *, #9221, .T. ) ;
#2518 = EDGE_CURVE ( 'NONE', #2409, #12158, #4374, .T. ) ;
#2519 = CIRCLE ( 'NONE', #11700, 0.3962400000000010358 ) ;
#2520 = CARTESIAN_POINT ( 'NONE',  ( 10.63496985936944483, -4.911985970482035668, -15.93575590714733536 ) ) ;
#2522 = CARTESIAN_POINT ( 'NONE',  ( 2.063750000000000195, 30.56064500000000095, -19.71675000000000111 ) ) ;
#2521 = CARTESIAN_POINT ( 'NONE',  ( 4.604894575570973814, 10.97102203747262195, 3.812269742438572973 ) ) ;
#2523 = AXIS2_PLACEMENT_3D ( 'NONE', #16109, #9012, #7687 ) ;
#2524 = VERTEX_POINT ( 'NONE', #13073 ) ;
#2525 = CARTESIAN_POINT ( 'NONE',  ( 3.513538848007559778, 15.00484000090286152, -1.245897553462994800 ) ) ;
#2526 = ORIENTED_EDGE ( 'NONE', *, *, #18854, .T. ) ;
#2527 = ORIENTED_EDGE ( 'NONE', *, *, #11249, .F. ) ;
#2528 = ORIENTED_EDGE ( 'NONE', *, *, #5424, .F. ) ;
#2529 = VECTOR ( 'NONE', #15760, 1000.000000000000000 ) ;
#2530 = VECTOR ( 'NONE', #16813, 1000.000000000000000 ) ;
#2531 = AXIS2_PLACEMENT_3D ( 'NONE', #4319, #887, #5854 ) ;
#2532 = CARTESIAN_POINT ( 'NONE',  ( 46.03750000000000142, 30.56064500000000095, -10.31874999999999964 ) ) ;
#2533 = DIRECTION ( 'NONE',  ( 0.9579671649362032637, 0.000000000000000000, -0.2868778675745010664 ) ) ;
#2534 = CARTESIAN_POINT ( 'NONE',  ( 1.952969610814715207, 23.80837275291289856, 8.731249999999999289 ) ) ;
#2535 = CARTESIAN_POINT ( 'NONE',  ( 54.61912012054379062, -6.356984999999999886, -13.79062155615056362 ) ) ;
#2536 = CARTESIAN_POINT ( 'NONE',  ( 3.227538363289882195, 11.94188570999173571, 6.753139928253237834 ) ) ;
#2537 = VERTEX_POINT ( 'NONE', #11399 ) ;
#2538 = CARTESIAN_POINT ( 'NONE',  ( 4.527065879313684427, 11.94740837896324237, 2.138596589892054034 ) ) ;
#2539 = CARTESIAN_POINT ( 'NONE',  ( 61.09555596642878328, 34.52875999999999834, -12.53419992421059348 ) ) ;
#2540 = CARTESIAN_POINT ( 'NONE',  ( -12.22950766483838336, -1.587500000000002132, -1.149759107507316580 ) ) ;
#2541 = CARTESIAN_POINT ( 'NONE',  ( -1.629142294184690698, 34.12394749999999988, -7.057664713974870274 ) ) ;
#2542 = ORIENTED_EDGE ( 'NONE', *, *, #1704, .T. ) ;
#2543 = EDGE_CURVE ( 'NONE', #10465, #9581, #14404, .T. ) ;
#2544 = ORIENTED_EDGE ( 'NONE', *, *, #10432, .T. ) ;
#2545 = CARTESIAN_POINT ( 'NONE',  ( 10.84552853021218688, 12.37556557019096282, -2.818576892710451531 ) ) ;
#2547 = CARTESIAN_POINT ( 'NONE',  ( 57.35354854712898742, -1.983739999999999837, -21.22263945788050776 ) ) ;
#2546 = CARTESIAN_POINT ( 'NONE',  ( 29.36874999999999858, 9.921875000000000000, 10.71562499999999929 ) ) ;
#2548 = CARTESIAN_POINT ( 'NONE',  ( 12.48372930177676920, 10.56671872245006050, 2.763668074036412570 ) ) ;
#2549 = VERTEX_POINT ( 'NONE', #11074 ) ;
#2550 = AXIS2_PLACEMENT_3D ( 'NONE', #7940, #4741, #2645 ) ;
#2551 = ORIENTED_EDGE ( 'NONE', *, *, #6778, .F. ) ;
#2552 = DIRECTION ( 'NONE',  ( 0.9685006480810793850, 0.000000000000000000, 0.2490110332224848011 ) ) ;
#2553 = AXIS2_PLACEMENT_3D ( 'NONE', #9600, #19557, #18127 ) ;
#2554 = CARTESIAN_POINT ( 'NONE',  ( 7.604625018144008486, 19.02913910763591687, -2.252239620500007256 ) ) ;
#2555 = CARTESIAN_POINT ( 'NONE',  ( 4.609813405446039347, 11.78043576488526156, 3.796358869022819604 ) ) ;
#2556 = CARTESIAN_POINT ( 'NONE',  ( 27.87822510359947614, 37.11476346399999926, -8.893823290944665061 ) ) ;
#2557 = CARTESIAN_POINT ( 'NONE',  ( 6.993363486292583531, 20.75028404412490701, 1.749401355466371433 ) ) ;
#2558 = VECTOR ( 'NONE', #21534, 1000.000000000000000 ) ;
#2559 = CIRCLE ( 'NONE', #1131, 0.3962399999999986488 ) ;
#2560 = CARTESIAN_POINT ( 'NONE',  ( 45.06824031473712466, -6.356984999999999886, -7.839138111891783112 ) ) ;
#2561 = CARTESIAN_POINT ( 'NONE',  ( 10.52032305797299649, 21.01595720978967918, 5.334914312547826221 ) ) ;
#2562 = DIRECTION ( 'NONE',  ( 0.000000000000000000, -1.000000000000000000, -0.000000000000000000 ) ) ;
#2563 = DIRECTION ( 'NONE',  ( 0.08420877549337300871, 0.000000000000000000, 0.9964481331860212121 ) ) ;
#2564 = DIRECTION ( 'NONE',  ( 0.000000000000000000, 1.000000000000000000, 0.000000000000000000 ) ) ;
#2565 = CARTESIAN_POINT ( 'NONE',  ( 4.055157505679755303, 21.31629319454957994, 5.262475580173261669 ) ) ;
#2566 = CARTESIAN_POINT ( 'NONE',  ( 1.087827283830285152, 11.64378971619068182, 6.276593309653182295 ) ) ;
#2567 = CARTESIAN_POINT ( 'NONE',  ( 38.82016491058538321, 0.000000000000000000, -14.75770094105646812 ) ) ;
#2568 = CARTESIAN_POINT ( 'NONE',  ( 4.515094011053506939, 19.87742190051230295, 6.403799425183819061 ) ) ;
#2569 = DIRECTION ( 'NONE',  ( 0.000000000000000000, 1.000000000000000000, 0.000000000000000000 ) ) ;
#2570 = CARTESIAN_POINT ( 'NONE',  ( 29.36874999999999858, 9.921875000000000000, 8.731249999999999289 ) ) ;
#2571 = CARTESIAN_POINT ( 'NONE',  ( 13.80933250118894229, 1.859310833520770867, -16.10574153504097694 ) ) ;
#2572 = ORIENTED_EDGE ( 'NONE', *, *, #14972, .F. ) ;
#2573 = CARTESIAN_POINT ( 'NONE',  ( 30.78626241496060700, -5.959792500000001603, -2.552201779827368622 ) ) ;
#2574 = EDGE_CURVE ( 'NONE', #6701, #19617, #20416, .T. ) ;
#2575 = AXIS2_PLACEMENT_3D ( 'NONE', #21716, #16432, #13116 ) ;
#2576 = CARTESIAN_POINT ( 'NONE',  ( 10.32109744938338736, 10.57878439573850216, 2.246271997629611050 ) ) ;
#2577 = VERTEX_POINT ( 'NONE', #8385 ) ;
#2578 = CARTESIAN_POINT ( 'NONE',  ( 23.76786555786699751, 0.8616843459004039918, 10.36815399131119975 ) ) ;
#2579 = CARTESIAN_POINT ( 'NONE',  ( 11.75421244062162707, 19.65546872379294641, -2.449785111124973547 ) ) ;
#2580 = CARTESIAN_POINT ( 'NONE',  ( 5.668659900314127142, 12.22025655502366170, -0.2948841661913189638 ) ) ;
#2581 = DIRECTION ( 'NONE',  ( 0.000000000000000000, 0.000000000000000000, 1.000000000000000000 ) ) ;
#2582 = CARTESIAN_POINT ( 'NONE',  ( 1.218075570542494157, 20.32969464963275996, 3.548942957621183503 ) ) ;
#2583 = VERTEX_POINT ( 'NONE', #1868 ) ;
#2584 = DIRECTION ( 'NONE',  ( 1.000000000000000000, 0.000000000000000000, 0.000000000000000000 ) ) ;
#2585 = AXIS2_PLACEMENT_3D ( 'NONE', #20791, #2680, #21025 ) ;
#2586 = PLANE ( 'NONE',  #16764 ) ;
#2587 = VERTEX_POINT ( 'NONE', #19994 ) ;
#2588 = CIRCLE ( 'NONE', #8234, 0.3962399999999990929 ) ;
#2589 = CARTESIAN_POINT ( 'NONE',  ( 11.52990124875157285, 14.00597049205862277, 6.372915746226297529 ) ) ;
#2590 = CARTESIAN_POINT ( 'NONE',  ( 12.45292882564249126, 11.21852838486178250, 2.551366500747729749 ) ) ;
#2591 = CARTESIAN_POINT ( 'NONE',  ( 201.9384738932629944, 1.983739999999999837, 8.731885000000000119 ) ) ;
#2592 = CARTESIAN_POINT ( 'NONE',  ( 31.83819605565793509, -1.983739999999999393, -4.158220719828246814 ) ) ;
#2593 = CARTESIAN_POINT ( 'NONE',  ( 53.25207718670083779, -7.553614316632189407, -16.53988246642675009 ) ) ;
#2594 = CARTESIAN_POINT ( 'NONE',  ( 19.84534036711146143, -1.573540299197002224, -15.46898262837090243 ) ) ;
#2595 = CARTESIAN_POINT ( 'NONE',  ( 3.615788786696767954, 21.36951672728427098, 4.012832544778790478 ) ) ;
#2596 = AXIS2_PLACEMENT_3D ( 'NONE', #1064, #6365, #13028 ) ;
#2597 = DIRECTION ( 'NONE',  ( -0.9943660382494290406, 0.000000000000000000, 0.1060008583745199739 ) ) ;
#2598 = EDGE_CURVE ( 'NONE', #17189, #7442, #7339, .T. ) ;
#2599 = VERTEX_POINT ( 'NONE', #4967 ) ;
#2600 = EDGE_CURVE ( 'NONE', #12951, #7504, #7908, .T. ) ;
#2601 = DIRECTION ( 'NONE',  ( -0.9685006480810794960, 0.000000000000000000, -0.2490110332224836354 ) ) ;
#2602 = EDGE_LOOP ( 'NONE', ( #11906, #1791, #11117, #1103 ) ) ;
#2603 = CARTESIAN_POINT ( 'NONE',  ( 10.02812634705811234, 19.92366122336811785, -1.416044127237466643 ) ) ;
#2604 = CARTESIAN_POINT ( 'NONE',  ( 26.59062499999999929, 26.59189500000000095, 8.731249999999999289 ) ) ;
#2605 = VECTOR ( 'NONE', #10573, 1000.000000000000000 ) ;
#2606 = CARTESIAN_POINT ( 'NONE',  ( 1.380668470443014995, 16.87825376251806020, 8.818428724692342513 ) ) ;
#2608 = DIRECTION ( 'NONE',  ( -0.000000000000000000, -1.000000000000000000, 0.000000000000000000 ) ) ;
#2607 = CARTESIAN_POINT ( 'NONE',  ( 1.061556958528351302, 17.24875406955469259, 9.359407947903699565 ) ) ;
#2609 = ORIENTED_EDGE ( 'NONE', *, *, #7352, .F. ) ;
#2610 = SHAPE_REPRESENTATION_RELATIONSHIP ( 'NONE' , 'NONE' ,  #3526, #6907 ) ;
#2611 = DIRECTION ( 'NONE',  ( 0.000000000000000000, -1.000000000000000000, 0.000000000000000000 ) ) ;
#2612 = CARTESIAN_POINT ( 'NONE',  ( 31.02798609601340729, 0.000000000000000000, -5.485920235548950252 ) ) ;
#2613 = ORIENTED_EDGE ( 'NONE', *, *, #11173, .F. ) ;
#2614 = CARTESIAN_POINT ( 'NONE',  ( -22.90765545213488963, 43.41875999999999891, -9.869178565316103047 ) ) ;
#2615 = VECTOR ( 'NONE', #17712, 1000.000000000000000 ) ;
#2616 = CARTESIAN_POINT ( 'NONE',  ( 19.93134302918909384, -1.593178467216436411, -15.39176060413034364 ) ) ;
#2617 = ORIENTED_EDGE ( 'NONE', *, *, #8323, .F. ) ;
#2618 = FACE_OUTER_BOUND ( 'NONE', #4833, .T. ) ;
#2619 = CARTESIAN_POINT ( 'NONE',  ( 1.911717863348795454, 16.21068983458730273, 0.06601438884004878771 ) ) ;
#2620 = EDGE_CURVE ( 'NONE', #6460, #19683, #14276, .T. ) ;
#2621 = CARTESIAN_POINT ( 'NONE',  ( 13.45807824676604625, 16.76891278191635593, 7.254207109304789292 ) ) ;
#2622 = VECTOR ( 'NONE', #2563, 1000.000000000000000 ) ;
#2623 = CARTESIAN_POINT ( 'NONE',  ( 29.03861462519914838, 16.26393749999999727, -4.929525984831418128 ) ) ;
#2624 = EDGE_CURVE ( 'NONE', #20381, #15906, #3647, .T. ) ;
#2625 = VERTEX_POINT ( 'NONE', #11609 ) ;
#2626 = ADVANCED_FACE ( 'NONE', ( #13390 ), #3327, .T. ) ;
#2627 = DIRECTION ( 'NONE',  ( 0.2490110332224850509, 0.000000000000000000, -0.9685006480810792739 ) ) ;
#2629 = CARTESIAN_POINT ( 'NONE',  ( 19.79515554403045741, -3.968114999999999615, -10.69562145279641996 ) ) ;
#2628 = CARTESIAN_POINT ( 'NONE',  ( 9.058884679750676128, -3.968114999999999615, -16.32319115207028659 ) ) ;
#2630 = AXIS2_PLACEMENT_3D ( 'NONE', #1300, #13045, #14375 ) ;
#2631 = EDGE_LOOP ( 'NONE', ( #6751, #20403, #16132, #5835 ) ) ;
#2632 = ORIENTED_EDGE ( 'NONE', *, *, #4378, .T. ) ;
#2633 = CARTESIAN_POINT ( 'NONE',  ( -14.45909654372175090, 36.51313499999967860, -9.781826438796489498 ) ) ;
#2635 = DIRECTION ( 'NONE',  ( 0.000000000000000000, 1.000000000000000000, 0.000000000000000000 ) ) ;
#2634 = CARTESIAN_POINT ( 'NONE',  ( 1.905042971753606373, 18.25238594264126135, -0.4688794665317326804 ) ) ;
#2636 = VERTEX_POINT ( 'NONE', #8612 ) ;
#2637 = CARTESIAN_POINT ( 'NONE',  ( 3.518382746470379185, 15.72191495716070797, -1.383387655830451868 ) ) ;
#2638 = ORIENTED_EDGE ( 'NONE', *, *, #10240, .F. ) ;
#2639 = EDGE_LOOP ( 'NONE', ( #4484, #9676, #15711, #14242 ) ) ;
#2640 = B_SPLINE_CURVE_WITH_KNOTS ( 'NONE', 3,
 ( #11793, #18526, #3391, #14017, #9009 ),
 .UNSPECIFIED., .F., .F.,
 ( 4, 1, 4 ),
 ( 0.003699823995551414398, 0.003727086906962521692, 0.003754349818373628987 ),
 .UNSPECIFIED. ) ;
#2641 = AXIS2_PLACEMENT_3D ( 'NONE', #818, #7341, #9202 ) ;
#2642 = ORIENTED_EDGE ( 'NONE', *, *, #15646, .F. ) ;
#2643 = EDGE_CURVE ( 'NONE', #5275, #11489, #6737, .T. ) ;
#2644 = TOROIDAL_SURFACE ( 'NONE', #4064, 3.174999999999999822, 1.190625000000000044 ) ;
#2645 = DIRECTION ( 'NONE',  ( 0.6702301885068632226, 0.000000000000000000, 0.7421532822901576454 ) ) ;
#2646 = PLANE ( 'NONE',  #13935 ) ;
#2647 = CARTESIAN_POINT ( 'NONE',  ( -46.55710204590916135, 41.43438499999999891, -7.870588902259476605 ) ) ;
#2648 = DIRECTION ( 'NONE',  ( 0.2227372614607789347, 0.000000000000000000, 0.9748785115884710528 ) ) ;
#2649 = CARTESIAN_POINT ( 'NONE',  ( 2.109114244753337086, 11.89287442835424713, 1.870778569916088152 ) ) ;
#2650 = ORIENTED_EDGE ( 'NONE', *, *, #6027, .T. ) ;
#2651 = DIRECTION ( 'NONE',  ( 0.000000000000000000, -1.000000000000000000, 0.000000000000000000 ) ) ;
#2652 = CARTESIAN_POINT ( 'NONE',  ( 49.28028498622276032, 32.54502000000000095, -25.68670502218146368 ) ) ;
#2653 = LINE ( 'NONE', #16150, #6790 ) ;
#2654 = DIRECTION ( 'NONE',  ( 0.000000000000000000, -1.000000000000000000, -0.000000000000000000 ) ) ;
#2655 = CARTESIAN_POINT ( 'NONE',  ( 42.27821610176829381, 32.54502000000000095, 7.496956594510385763 ) ) ;
#2656 = ORIENTED_EDGE ( 'NONE', *, *, #1137, .F. ) ;
#2657 = ORIENTED_EDGE ( 'NONE', *, *, #3846, .T. ) ;
#2658 = CARTESIAN_POINT ( 'NONE',  ( 7.895845287764687193, 11.40205806595764138, 1.929403598022860544 ) ) ;
#2660 = CARTESIAN_POINT ( 'NONE',  ( 39.16413618835606769, 0.000000000000000000, -24.45043885672975392 ) ) ;
#2659 = LINE ( 'NONE', #18016, #14030 ) ;
#2661 = CARTESIAN_POINT ( 'NONE',  ( 11.81437950571842421, 10.58622871606461224, -0.01149372372624126934 ) ) ;
#2662 = EDGE_LOOP ( 'NONE', ( #6177, #3400, #13676, #18605 ) ) ;
#2663 = VECTOR ( 'NONE', #20289, 1000.000000000000000 ) ;
#2664 = ORIENTED_EDGE ( 'NONE', *, *, #21131, .F. ) ;
#2665 = PLANE ( 'NONE',  #14862 ) ;
#2666 = CARTESIAN_POINT ( 'NONE',  ( 8.008853420312213700, 10.95545630081279143, 1.083615874370668752 ) ) ;
#2667 = CARTESIAN_POINT ( 'NONE',  ( 8.666075731349446087, 19.39233966230795403, 6.124975956293988943 ) ) ;
#2668 = CARTESIAN_POINT ( 'NONE',  ( 2.553282444597012368, 19.73155930485265586, 6.734093347788381756 ) ) ;
#2669 = CARTESIAN_POINT ( 'NONE',  ( 55.27198911326564001, 0.000000000000000000, 2.462719476673013830 ) ) ;
#2670 = ADVANCED_FACE ( 'NONE', ( #5181 ), #5086, .T. ) ;
#2671 = ADVANCED_FACE ( 'NONE', ( #18663 ), #10160, .F. ) ;
#2672 = CARTESIAN_POINT ( 'NONE',  ( 7.473677272119537029, 12.62524416591024057, -1.682421981746856865 ) ) ;
#2673 = B_SPLINE_CURVE_WITH_KNOTS ( 'NONE', 3,
 ( #19929, #11532, #7994, #19704 ),
 .UNSPECIFIED., .F., .F.,
 ( 4, 4 ),
 ( -7.968845587668896464E-05, 0.0005317181549816462575 ),
 .UNSPECIFIED. ) ;
#2674 = AXIS2_PLACEMENT_3D ( 'NONE', #14768, #6332, #21592 ) ;
#2675 = CARTESIAN_POINT ( 'NONE',  ( 13.57150076887395151, 22.11904549731909952, 1.890065446233673452 ) ) ;
#2676 = DIRECTION ( 'NONE',  ( 0.000000000000000000, 1.000000000000000000, 0.000000000000000000 ) ) ;
#2677 = DIRECTION ( 'NONE',  ( 0.000000000000000000, 1.000000000000000000, 0.000000000000000000 ) ) ;
#2678 = CARTESIAN_POINT ( 'NONE',  ( 3.582999334761938659, 17.35319764795464792, -1.443157694066694807 ) ) ;
#2679 = CARTESIAN_POINT ( 'NONE',  ( 1.136769403771278775, 11.72606752483194192, 6.493935939501890076 ) ) ;
#2680 = DIRECTION ( 'NONE',  ( -1.000000000000000000, 0.000000000000000000, 0.000000000000000000 ) ) ;
#2681 = CARTESIAN_POINT ( 'NONE',  ( -0.2158892827208123977, 20.30256849354482185, 4.809740601404282501 ) ) ;
#2682 = CARTESIAN_POINT ( 'NONE',  ( -47.86049599909252805, 41.43438499999999891, -23.29373766372935961 ) ) ;
#2683 = CARTESIAN_POINT ( 'NONE',  ( 20.38332674228396613, -1.359449706705494920, -15.33066107936057065 ) ) ;
#2684 = CARTESIAN_POINT ( 'NONE',  ( 11.97511817037405812, -6.853367414429714977, -15.72877504999935283 ) ) ;
#2685 = ORIENTED_EDGE ( 'NONE', *, *, #18562, .F. ) ;
#2686 = DIRECTION ( 'NONE',  ( 0.3447671952293626108, 0.000000000000000000, 0.9386882235831439658 ) ) ;
#2687 = CARTESIAN_POINT ( 'NONE',  ( 9.742485288642992458, 11.02108255535072168, -0.1776678401114160366 ) ) ;
#2688 = ORIENTED_EDGE ( 'NONE', *, *, #21779, .F. ) ;
#2689 = CARTESIAN_POINT ( 'NONE',  ( 53.25483508941461963, -9.531985000000000596, -5.879799058943532941 ) ) ;
#2690 = CARTESIAN_POINT ( 'NONE',  ( 12.54102569310331816, 21.14438424194486288, -0.3961202071941773983 ) ) ;
#2691 = CARTESIAN_POINT ( 'NONE',  ( 5.644721527306630016, 12.32188619433131294, -0.4059770778182363316 ) ) ;
#2692 = DIRECTION ( 'NONE',  ( 1.000000000000000000, 0.000000000000000000, 0.000000000000000000 ) ) ;
#2693 = CARTESIAN_POINT ( 'NONE',  ( 5.111570728101542116, 12.95486688907394246, 6.687046794338158406 ) ) ;
#2694 = EDGE_LOOP ( 'NONE', ( #281, #4609, #228, #6807 ) ) ;
#2695 = DIRECTION ( 'NONE',  ( 0.6050250551579484659, -0.7753173868113210077, -0.1811839737371541414 ) ) ;
#2696 = EDGE_CURVE ( 'NONE', #12008, #9848, #10059, .T. ) ;
#2697 = CARTESIAN_POINT ( 'NONE',  ( 11.41393435462807737, 17.53555608635337393, 6.774740267079724987 ) ) ;
#2698 = CARTESIAN_POINT ( 'NONE',  ( 5.005774954510405550, 18.45579612835071615, 7.507356342279577710 ) ) ;
#2699 = DIRECTION ( 'NONE',  ( 0.000000000000000000, 1.000000000000000000, 0.000000000000000000 ) ) ;
#2700 = DIRECTION ( 'NONE',  ( 0.000000000000000000, 1.000000000000000000, 0.000000000000000000 ) ) ;
#2701 = CARTESIAN_POINT ( 'NONE',  ( 19.84450919603384733, -1.527652306611041233, -14.98753281959816874 ) ) ;
#2702 = DIRECTION ( 'NONE',  ( 0.000000000000000000, 1.000000000000000000, 0.000000000000000000 ) ) ;
#2703 = FACE_BOUND ( 'NONE', #11148, .T. ) ;
#2704 = DIRECTION ( 'NONE',  ( -0.9959941601142525691, 0.000000000000000000, -0.08941830359777946935 ) ) ;
#2705 = VERTEX_POINT ( 'NONE', #15388 ) ;
#2706 = CARTESIAN_POINT ( 'NONE',  ( 17.30373842852263877, 36.51313500000000545, -12.15706637069277107 ) ) ;
#2707 = CARTESIAN_POINT ( 'NONE',  ( 30.78626241496060700, 30.54508749999999750, -2.552201779827368622 ) ) ;
#2708 = EDGE_LOOP ( 'NONE', ( #17112, #5494, #20962, #13650, #10840, #11675, #14095 ) ) ;
#2709 = CARTESIAN_POINT ( 'NONE',  ( 11.97400483195221277, 20.77626866726145138, 3.770676366985183936 ) ) ;
#2710 = CARTESIAN_POINT ( 'NONE',  ( 1.140921941160975228, 18.20957084091965683, 8.407057880873713529 ) ) ;
#2711 = CARTESIAN_POINT ( 'NONE',  ( 11.33771398496533855, 0.1030544890320075901, -16.36893042155433875 ) ) ;
#2713 = DIRECTION ( 'NONE',  ( 0.000000000000000000, 1.000000000000000000, 0.000000000000000000 ) ) ;
#2712 = CARTESIAN_POINT ( 'NONE',  ( 4.163765799268428047, 11.37607716600946084, 3.937147338019182374 ) ) ;
#2714 = VERTEX_POINT ( 'NONE', #4866 ) ;
#2715 =( NAMED_UNIT ( * ) SI_UNIT ( $, .STERADIAN. ) SOLID_ANGLE_UNIT ( ) );
#2716 = CARTESIAN_POINT ( 'NONE',  ( 1.954387715434429795, 8.736780638212259475, 10.71562499999999929 ) ) ;
#2717 = FACE_OUTER_BOUND ( 'NONE', #21076, .T. ) ;
#2718 = ORIENTED_EDGE ( 'NONE', *, *, #237, .F. ) ;
#2719 = CARTESIAN_POINT ( 'NONE',  ( 19.49278356037279991, -0.05523789353248333145, -15.00694009703612686 ) ) ;
#2720 = EDGE_CURVE ( 'NONE', #13936, #5560, #17797, .T. ) ;
#2721 = CARTESIAN_POINT ( 'NONE',  ( 17.19235063062528468, -7.334996653170583691, -15.79220656676793411 ) ) ;
#2722 = VERTEX_POINT ( 'NONE', #15278 ) ;
#2723 = CARTESIAN_POINT ( 'NONE',  ( 8.556880530951183061, 11.53658052784436094, 3.544415608734076351 ) ) ;
#2724 = CARTESIAN_POINT ( 'NONE',  ( 2.476689525297502747, 19.21360138094522796, 1.103912187563293790 ) ) ;
#2725 = CARTESIAN_POINT ( 'NONE',  ( 9.457138866168421032, 16.63237982350910826, 8.096441382392347563 ) ) ;
#2726 = CIRCLE ( 'NONE', #14759, 1.190624999999997824 ) ;
#2727 = FACE_OUTER_BOUND ( 'NONE', #524, .T. ) ;
#2728 = ORIENTED_EDGE ( 'NONE', *, *, #10631, .T. ) ;
#2729 = CARTESIAN_POINT ( 'NONE',  ( 14.25617145423489696, -3.968114999999999615, -15.80779474975094168 ) ) ;
#2730 = CARTESIAN_POINT ( 'NONE',  ( 18.11264938600108820, 5.747448040522750823, -19.32386823132846132 ) ) ;
#2731 = VERTEX_POINT ( 'NONE', #13614 ) ;
#2732 = VERTEX_POINT ( 'NONE', #20098 ) ;
#2733 = CARTESIAN_POINT ( 'NONE',  ( 1.854799496439154316, 19.43893749999999798, 3.211081754263136911 ) ) ;
#2735 = CARTESIAN_POINT ( 'NONE',  ( 61.81956123787853130, -1.983739999999999837, -1.238102447480925239 ) ) ;
#2734 = CARTESIAN_POINT ( 'NONE',  ( 6.010155830883637584, 11.27374497607938331, 1.140174849044627070 ) ) ;
#2736 = ORIENTED_EDGE ( 'NONE', *, *, #2262, .T. ) ;
#2737 = CARTESIAN_POINT ( 'NONE',  ( 3.536137602566534532, 16.20739087061626194, -1.426542626591323693 ) ) ;
#2738 = EDGE_CURVE ( 'NONE', #19531, #3414, #6496, .T. ) ;
#2739 = ORIENTED_EDGE ( 'NONE', *, *, #1751, .T. ) ;
#2740 = AXIS2_PLACEMENT_3D ( 'NONE', #1315, #13281, #15050 ) ;
#2741 = EDGE_LOOP ( 'NONE', ( #14917, #640, #16235, #11591 ) ) ;
#2742 = EDGE_CURVE ( 'NONE', #2587, #5690, #11932, .T. ) ;
#2743 = VERTEX_POINT ( 'NONE', #9947 ) ;
#2744 = EDGE_CURVE ( 'NONE', #10152, #13027, #2977, .T. ) ;
#2745 = EDGE_CURVE ( 'NONE', #18449, #5398, #21668, .T. ) ;
#2746 = PLANE ( 'NONE',  #10678 ) ;
#2747 = FACE_OUTER_BOUND ( 'NONE', #9626, .T. ) ;
#2748 = DIRECTION ( 'NONE',  ( 0.08420877549337300871, 0.000000000000000000, 0.9964481331860212121 ) ) ;
#2749 = CARTESIAN_POINT ( 'NONE',  ( 30.41963056417667488, 34.52875999999999834, -8.653862521447852174 ) ) ;
#2750 = CARTESIAN_POINT ( 'NONE',  ( 3.051292505765481611, 11.56282819984068233, 5.969449698946827532 ) ) ;
#2751 = AXIS2_PLACEMENT_3D ( 'NONE', #1328, #21561, #13077 ) ;
#2752 = EDGE_LOOP ( 'NONE', ( #2617, #17130, #21168, #2517, #13607, #11181 ) ) ;
#2753 = LINE ( 'NONE', #18229, #11053 ) ;
#2754 = CARTESIAN_POINT ( 'NONE',  ( 30.78626241496060700, 30.50833916023545811, -2.552201779827368622 ) ) ;
#2755 = CARTESIAN_POINT ( 'NONE',  ( 13.21598617904356843, 21.40926851296702438, 1.892361481066431761 ) ) ;
#2756 = PRESENTATION_STYLE_ASSIGNMENT (( #12949 ) ) ;
#2757 = ORIENTED_EDGE ( 'NONE', *, *, #13924, .F. ) ;
#2758 = EDGE_LOOP ( 'NONE', ( #819, #5356, #9094, #1296 ) ) ;
#2759 = CARTESIAN_POINT ( 'NONE',  ( 7.245293160062258764, 13.09203250846072208, -1.032046942138396428 ) ) ;
#2761 = CARTESIAN_POINT ( 'NONE',  ( -12.30312499999999964, 1.984057500000000251, 10.71562499999999929 ) ) ;
#2760 = DIRECTION ( 'NONE',  ( 0.9964481331860213231, 0.000000000000000000, -0.08420877549337293932 ) ) ;
#2762 = CARTESIAN_POINT ( 'NONE',  ( 10.92596818984666740, 15.71281552240790980, -4.318717355501334509 ) ) ;
#2763 = ORIENTED_EDGE ( 'NONE', *, *, #9397, .T. ) ;
#2764 = EDGE_CURVE ( 'NONE', #8452, #12517, #10390, .T. ) ;
#2765 = ORIENTED_EDGE ( 'NONE', *, *, #19882, .T. ) ;
#2766 = CARTESIAN_POINT ( 'NONE',  ( 11.42842559562532578, -1.983739999999999393, 1.673196738795719174 ) ) ;
#2767 = CARTESIAN_POINT ( 'NONE',  ( 8.082574189534248887, 20.56981455947430248, -1.053435052150081708 ) ) ;
#2768 = CARTESIAN_POINT ( 'NONE',  ( 8.985952281912938489, 18.19521758435699965, 6.854078172061496943 ) ) ;
#2769 = AXIS2_PLACEMENT_3D ( 'NONE', #10291, #10413, #18685 ) ;
#2770 = EDGE_CURVE ( 'NONE', #7013, #4043, #15933, .T. ) ;
#2771 = CARTESIAN_POINT ( 'NONE',  ( 2.772268972823688227, 19.27421045831329138, 7.270480256298323951 ) ) ;
#2772 = DIRECTION ( 'NONE',  ( 0.2490110332224850231, 0.000000000000000000, -0.9685006480810791629 ) ) ;
#2773 = AXIS2_PLACEMENT_3D ( 'NONE', #4907, #11449, #6672 ) ;
#2774 = CARTESIAN_POINT ( 'NONE',  ( -13.49374999999999858, 0.000000000000000000, 0.000000000000000000 ) ) ;
#2775 = DIRECTION ( 'NONE',  ( -0.000000000000000000, -1.000000000000000000, 0.000000000000000000 ) ) ;
#2776 = CARTESIAN_POINT ( 'NONE',  ( 3.515085772594902291, 13.11399658182230077, 8.225784691290757067 ) ) ;
#2777 = CARTESIAN_POINT ( 'NONE',  ( 0.8915019007142239715, 11.45163104751902239, 5.416119751115242131 ) ) ;
#2778 = EDGE_LOOP ( 'NONE', ( #21084, #5570, #15508, #2989 ) ) ;
#2779 = CARTESIAN_POINT ( 'NONE',  ( 1.951530046808849228, 14.88544593074506928, 0.2113062994974087283 ) ) ;
#2780 = PLANE ( 'NONE',  #4942 ) ;
#2781 = FACE_OUTER_BOUND ( 'NONE', #14172, .T. ) ;
#2782 = CARTESIAN_POINT ( 'NONE',  ( 11.87758290844151787, -6.747997337208533786, -15.74855984373561135 ) ) ;
#2783 = ORIENTED_EDGE ( 'NONE', *, *, #20016, .T. ) ;
#2784 = PLANE ( 'NONE',  #9934 ) ;
#2785 = AXIS2_PLACEMENT_3D ( 'NONE', #5633, #2209, #12059 ) ;
#2786 = CARTESIAN_POINT ( 'NONE',  ( 9.284756493703616442, 12.52235313574567144, -2.202660405334921023 ) ) ;
#2787 = ORIENTED_EDGE ( 'NONE', *, *, #15032, .F. ) ;
#2788 = EDGE_CURVE ( 'NONE', #1096, #20725, #5083, .T. ) ;
#2789 = CARTESIAN_POINT ( 'NONE',  ( 27.48935845518379750, 1.313173473011783887, 10.59903018670800101 ) ) ;
#2790 = EDGE_CURVE ( 'NONE', #19275, #2434, #17464, .T. ) ;
#2791 = EDGE_CURVE ( 'NONE', #8452, #7807, #20762, .T. ) ;
#2792 = CARTESIAN_POINT ( 'NONE',  ( 5.766733102981766557, 11.86842019456400621, 0.1504060388216716393 ) ) ;
#2793 = CYLINDRICAL_SURFACE ( 'NONE', #8442, 6.350000000000001421 ) ;
#2794 = CARTESIAN_POINT ( 'NONE',  ( 7.156415711929009937, 13.47382733369860119, 6.808263970100831841 ) ) ;
#2795 = ORIENTED_EDGE ( 'NONE', *, *, #15047, .T. ) ;
#2796 = VECTOR ( 'NONE', #4237, 1000.000000000000114 ) ;
#2797 = DIRECTION ( 'NONE',  ( 0.000000000000000000, 1.000000000000000000, 0.000000000000000000 ) ) ;
#2798 = CARTESIAN_POINT ( 'NONE',  ( 5.774898037902874037, 20.68996510477920836, 4.127828386637749425 ) ) ;
#2799 = CARTESIAN_POINT ( 'NONE',  ( 24.26606285357373594, 2.770822500000000854, -16.92219937337620195 ) ) ;
#2800 = AXIS2_PLACEMENT_3D ( 'NONE', #770, #17474, #9053 ) ;
#2801 = DIRECTION ( 'NONE',  ( 0.7421532822901579785, 0.000000000000000000, -0.6702301885068628895 ) ) ;
#2802 = CARTESIAN_POINT ( 'NONE',  ( 14.01242225938494457, 20.92405235932746166, 3.318798650793908678 ) ) ;
#2803 = CARTESIAN_POINT ( 'NONE',  ( 0.7655485048701912154, 20.32785531569650317, 1.774472875170517439 ) ) ;
#2804 = FACE_OUTER_BOUND ( 'NONE', #2847, .T. ) ;
#2805 = VECTOR ( 'NONE', #6594, 1000.000000000000000 ) ;
#2806 = CARTESIAN_POINT ( 'NONE',  ( 6.722594236988291172, 11.51780469952192298, 2.735504111625294943 ) ) ;
#2807 = DIRECTION ( 'NONE',  ( 0.000000000000000000, 1.000000000000000000, 0.000000000000000000 ) ) ;
#2808 = DIRECTION ( 'NONE',  ( -0.2490110332224857170, 0.000000000000000000, 0.9685006480810790519 ) ) ;
#2809 = AXIS2_PLACEMENT_3D ( 'NONE', #8306, #1241, #18362 ) ;
#2810 = CARTESIAN_POINT ( 'NONE',  ( 46.03750000000000142, 0.000000000000000000, -10.31874999999999964 ) ) ;
#2811 = ORIENTED_EDGE ( 'NONE', *, *, #1979, .T. ) ;
#2812 = CARTESIAN_POINT ( 'NONE',  ( 9.262381024405307528, 30.63641399982339308, -21.59935919086856515 ) ) ;
#2813 = CARTESIAN_POINT ( 'NONE',  ( 20.07205047641097551, 0.5575362955879438198, -14.29572329288908605 ) ) ;
#2814 = CARTESIAN_POINT ( 'NONE',  ( 11.56192577415882816, 36.51313500000000545, 4.677561850332325299 ) ) ;
#2815 = ORIENTED_EDGE ( 'NONE', *, *, #14864, .F. ) ;
#2816 = EDGE_CURVE ( 'NONE', #8109, #11708, #15601, .T. ) ;
#2817 = CARTESIAN_POINT ( 'NONE',  ( 11.47061170363800819, 21.20994850999973380, 2.421414491514969569 ) ) ;
#2818 = CARTESIAN_POINT ( 'NONE',  ( 1.481718377196148406, 15.01894485712453076, 8.639932247213000238 ) ) ;
#2819 = CARTESIAN_POINT ( 'NONE',  ( 17.77130180500099144, -8.167753660192959231, -13.99236777178278146 ) ) ;
#2821 = DIRECTION ( 'NONE',  ( 0.9997303917939455165, 0.000000000000000000, 0.02321946863139149123 ) ) ;
#2820 = CARTESIAN_POINT ( 'NONE',  ( -0.1178366066227022335, 13.07040487695864250, 2.210290218837267506 ) ) ;
#2822 = VERTEX_POINT ( 'NONE', #14277 ) ;
#2823 = LINE ( 'NONE', #7794, #3572 ) ;
#2824 = LINE ( 'NONE', #1370, #15156 ) ;
#2825 = ORIENTED_EDGE ( 'NONE', *, *, #14435, .T. ) ;
#2826 = VECTOR ( 'NONE', #20288, 1000.000000000000000 ) ;
#2827 = CARTESIAN_POINT ( 'NONE',  ( 20.11644828361683324, -1.217489419619933066, -14.78816586879083772 ) ) ;
#2828 = CARTESIAN_POINT ( 'NONE',  ( 0.5545849870865751097, 18.94100205338251186, 1.657181427631677417 ) ) ;
#2829 = CIRCLE ( 'NONE', #8461, 22.02656249999999005 ) ;
#2830 = ORIENTED_EDGE ( 'NONE', *, *, #18151, .F. ) ;
#2831 = CARTESIAN_POINT ( 'NONE',  ( 5.943860589180493648, 18.80374057110937969, -0.8413134284775921623 ) ) ;
#2832 = CARTESIAN_POINT ( 'NONE',  ( 2.480011849002778046, 19.22266723186190518, 1.111811738353578605 ) ) ;
#2833 = CARTESIAN_POINT ( 'NONE',  ( 12.61503648570790048, 20.52417811251926238, 5.621890414035338956 ) ) ;
#2834 = VECTOR ( 'NONE', #18906, 1000.000000000000000 ) ;
#2835 = CYLINDRICAL_SURFACE ( 'NONE', #11310, 0.3962399999999988154 ) ;
#2836 = ORIENTED_EDGE ( 'NONE', *, *, #21101, .T. ) ;
#2837 = VECTOR ( 'NONE', #474, 1000.000000000000114 ) ;
#2838 = CARTESIAN_POINT ( 'NONE',  ( 0.02083138522551555155, 20.24316500000000119, 7.210477125664100484 ) ) ;
#2839 = PLANE ( 'NONE',  #19092 ) ;
#2840 = ORIENTED_EDGE ( 'NONE', *, *, #10744, .F. ) ;
#2841 = ORIENTED_EDGE ( 'NONE', *, *, #11647, .T. ) ;
#2842 = ADVANCED_FACE ( 'NONE', ( #12165 ), #5623, .F. ) ;
#2843 = LINE ( 'NONE', #2733, #12 ) ;
#2844 = B_SPLINE_CURVE_WITH_KNOTS ( 'NONE', 3,
 ( #3264, #11656, #18502, #15325, #15432, #13336, #8337 ),
 .UNSPECIFIED., .F., .F.,
 ( 4, 1, 1, 1, 4 ),
 ( 0.000000000000000000, 0.2499992835874668695, 0.4999999879860682617, 0.7500006923846697093, 1.000000000000000000 ),
 .UNSPECIFIED. ) ;
#2846 = DIRECTION ( 'NONE',  ( 0.3542738219355897056, 0.000000000000000000, 0.9351417320872542627 ) ) ;
#2845 = CARTESIAN_POINT ( 'NONE',  ( 1.062432521211429393, 11.63297050342826289, 6.580026358220900207 ) ) ;
#2847 = EDGE_LOOP ( 'NONE', ( #13729, #21082, #4101, #13970 ) ) ;
#2848 = CARTESIAN_POINT ( 'NONE',  ( 3.856869842080445920, 12.13100849778645340, 0.6426578681662645787 ) ) ;
#2849 = ORIENTED_EDGE ( 'NONE', *, *, #4636, .T. ) ;
#2850 = CIRCLE ( 'NONE', #15217, 1.984374999999998890 ) ;
#2851 = ORIENTED_EDGE ( 'NONE', *, *, #17729, .T. ) ;
#2852 = ORIENTED_EDGE ( 'NONE', *, *, #13364, .T. ) ;
#2853 = VECTOR ( 'NONE', #17639, 1000.000000000000114 ) ;
#2854 = AXIS2_PLACEMENT_3D ( 'NONE', #11762, #13536, #10529 ) ;
#2855 = CARTESIAN_POINT ( 'NONE',  ( 4.073379047215689219, 12.50506245289733620, 1.480859224242744299 ) ) ;
#2856 = B_SPLINE_CURVE_WITH_KNOTS ( 'NONE', 3,
 ( #20566, #5428, #12193, #10638, #1222, #11281, #18145, #19780, #1110, #4334, #19578, #4654, #18029, #11176, #6195, #16488, #9618, #9726, #17829, #19673, #17928, #2675, #12740, #6298, #9405, #16384 ),
 .UNSPECIFIED., .F., .F.,
 ( 4, 2, 2, 1, 2, 2, 2, 2, 1, 2, 2, 2, 2, 4 ),
 ( 0.000000000000000000, 0.06249999999999787670, 0.1249999999999957534, 0.1874999999999936162, 0.2187499999999944489, 0.2499999999999952816, 0.5000000000000145439, 0.6250000000000203171, 0.6875000000000225375, 0.7187500000000225375, 0.7500000000000225375, 0.8125000000000168754, 0.8750000000000112133, 1.000000000000000000 ),
 .UNSPECIFIED. ) ;
#2857 = CARTESIAN_POINT ( 'NONE',  ( 12.91596452321051558, 12.29391749999999739, 2.799331278665067479 ) ) ;
#2858 = LINE ( 'NONE', #19869, #10037 ) ;
#2859 = AXIS2_PLACEMENT_3D ( 'NONE', #17284, #18934, #5675 ) ;
#2860 = CARTESIAN_POINT ( 'NONE',  ( -16.07247711516169275, -5.309201820043501385, -10.44681224123558039 ) ) ;
#2861 = DIRECTION ( 'NONE',  ( 1.000000000000000000, 0.000000000000000000, 0.000000000000000000 ) ) ;
#2862 = CARTESIAN_POINT ( 'NONE',  ( 3.270378689765827573, 12.06369702427301505, 6.947417772566477190 ) ) ;
#2863 = ORIENTED_EDGE ( 'NONE', *, *, #3055, .T. ) ;
#2864 = AXIS2_PLACEMENT_3D ( 'NONE', #5931, #9034, #1071 ) ;
#2865 = DIRECTION ( 'NONE',  ( 0.9636276526537417286, 0.000000000000000000, -0.2672484743474500268 ) ) ;
#2866 = DIRECTION ( 'NONE',  ( 0.000000000000000000, 1.000000000000000000, 0.000000000000000000 ) ) ;
#2867 = DIRECTION ( 'NONE',  ( -0.07875956036501312318, 0.000000000000000000, 0.9968936410927243807 ) ) ;
#2868 = DIRECTION ( 'NONE',  ( 0.2490110332224848289, 0.000000000000000000, -0.9685006480810792739 ) ) ;
#2869 = CARTESIAN_POINT ( 'NONE',  ( 66.87634738983680904, 32.54502000000000095, 3.497859541731999755 ) ) ;
#2870 = EDGE_LOOP ( 'NONE', ( #14960, #15454, #8532, #8925 ) ) ;
#2871 = ORIENTED_EDGE ( 'NONE', *, *, #992, .F. ) ;
#2872 = EDGE_CURVE ( 'NONE', #12131, #20877, #1197, .T. ) ;
#2873 = CARTESIAN_POINT ( 'NONE',  ( 9.804971849761239255, 20.33297925226851888, -1.164330711434534038 ) ) ;
#2874 = EDGE_CURVE ( 'NONE', #5388, #3524, #19220, .T. ) ;
#2876 = DIRECTION ( 'NONE',  ( 0.000000000000000000, -1.000000000000000000, -0.000000000000000000 ) ) ;
#2875 = CARTESIAN_POINT ( 'NONE',  ( 30.10940225190841701, 2.809619014187358932, -2.349505688218141319 ) ) ;
#2877 = CARTESIAN_POINT ( 'NONE',  ( 11.19677005946078552, 12.16295462910996150, -2.669674531000855833 ) ) ;
#2878 = ORIENTED_EDGE ( 'NONE', *, *, #1009, .T. ) ;
#2879 = AXIS2_PLACEMENT_3D ( 'NONE', #584, #4344, #8978 ) ;
#2880 = ORIENTED_EDGE ( 'NONE', *, *, #13843, .T. ) ;
#2881 = DIRECTION ( 'NONE',  ( 0.000000000000000000, 1.000000000000000000, 0.000000000000000000 ) ) ;
#2882 = CARTESIAN_POINT ( 'NONE',  ( 8.636160761027110055, 19.47637978834870154, 6.052143982077559770 ) ) ;
#2883 = AXIS2_PLACEMENT_3D ( 'NONE', #361, #12308, #10651 ) ;
#2884 = CIRCLE ( 'NONE', #1465, 1.190625000000000711 ) ;
#2885 = CIRCLE ( 'NONE', #21227, 1.190625000000000711 ) ;
#2886 = ADVANCED_FACE ( 'NONE', ( #20650 ), #759, .T. ) ;
#2887 = CARTESIAN_POINT ( 'NONE',  ( -15.39353573898878658, 37.13217763270220217, -10.30107656633069979 ) ) ;
#2888 = CARTESIAN_POINT ( 'NONE',  ( 29.98909767165928386, 38.48766750000000059, -5.214162619065493054 ) ) ;
#2889 = CARTESIAN_POINT ( 'NONE',  ( 6.698225881633547374, 10.91861244885538085, 4.257383380063560097 ) ) ;
#2890 = CARTESIAN_POINT ( 'NONE',  ( 1.494793067313823220, 12.79616285387843178, 8.147785873054054662 ) ) ;
#2891 = CARTESIAN_POINT ( 'NONE',  ( -14.35397337327049172, 34.31794000000000011, -0.6462872510839714479 ) ) ;
#2892 = EDGE_LOOP ( 'NONE', ( #18348, #7290, #17455, #8127 ) ) ;
#2893 = CARTESIAN_POINT ( 'NONE',  ( 4.219720171048965796, 12.02975038249582163, 2.261177325983976694 ) ) ;
#2894 = FACE_OUTER_BOUND ( 'NONE', #10046, .T. ) ;
#2895 = CARTESIAN_POINT ( 'NONE',  ( 1.854799496439154316, 13.08893749999999834, 3.211081754263136911 ) ) ;
#2896 = CARTESIAN_POINT ( 'NONE',  ( 20.18965527659050707, -5.828461386187921534, -13.97265621264273250 ) ) ;
#2897 = ORIENTED_EDGE ( 'NONE', *, *, #21417, .T. ) ;
#2898 = DIRECTION ( 'NONE',  ( 0.000000000000000000, 1.000000000000000000, 0.000000000000000000 ) ) ;
#2899 = CIRCLE ( 'NONE', #15272, 1.190625000000000711 ) ;
#2900 = CARTESIAN_POINT ( 'NONE',  ( 8.998936210029770066, 21.96122921384184323, 1.701528532610274702 ) ) ;
#2901 = EDGE_CURVE ( 'NONE', #119, #2583, #8256, .T. ) ;
#2902 = CARTESIAN_POINT ( 'NONE',  ( 10.07729208704005686, 20.97526076903321979, -1.393227384962903548 ) ) ;
#2903 = ORIENTED_EDGE ( 'NONE', *, *, #20412, .T. ) ;
#2904 = DIRECTION ( 'NONE',  ( 0.000000000000000000, -1.000000000000000000, -0.000000000000000000 ) ) ;
#2905 = CIRCLE ( 'NONE', #17744, 9.524999999999998579 ) ;
#2906 = CARTESIAN_POINT ( 'NONE',  ( 12.86658186011742799, 21.36847253319938034, 0.4848128236591797702 ) ) ;
#2907 = CARTESIAN_POINT ( 'NONE',  ( 8.526560839306522865, 20.68998476507356798, 5.890721982252703270 ) ) ;
#2908 = AXIS2_PLACEMENT_3D ( 'NONE', #10400, #4976, #1760 ) ;
#2909 = CYLINDRICAL_SURFACE ( 'NONE', #8787, 30.16250000000000497 ) ;
#2910 = CARTESIAN_POINT ( 'NONE',  ( 6.593701308395895744, 19.51815128457440451, 6.507342028609568452 ) ) ;
#2911 = CARTESIAN_POINT ( 'NONE',  ( 61.04701390398659555, 32.54502000000000095, -15.15157976445104993 ) ) ;
#2912 = EDGE_CURVE ( 'NONE', #8949, #12158, #4083, .T. ) ;
#2913 = CARTESIAN_POINT ( 'NONE',  ( 6.288807527935679431, 20.20918138442159773, 5.471213349970711626 ) ) ;
#2914 = DIRECTION ( 'NONE',  ( 0.000000000000000000, 1.000000000000000000, 0.000000000000000000 ) ) ;
#2915 = CIRCLE ( 'NONE', #8912, 4.961572499999999941 ) ;
#2916 = DIRECTION ( 'NONE',  ( 0.000000000000000000, 1.000000000000000000, 0.000000000000000000 ) ) ;
#2917 = CARTESIAN_POINT ( 'NONE',  ( 11.43683134601739049, 18.10558555415017068, -3.440669360032733604 ) ) ;
#2918 = CARTESIAN_POINT ( 'NONE',  ( 5.318399099313155354, 16.52349172687392098, 8.034301819513165910 ) ) ;
#2919 = EDGE_CURVE ( 'NONE', #1535, #2096, #11089, .T. ) ;
#2920 = DIRECTION ( 'NONE',  ( 0.000000000000000000, -1.000000000000000000, 0.000000000000000000 ) ) ;
#2921 = CARTESIAN_POINT ( 'NONE',  ( 7.017766547708233382, 11.00346980177178224, 4.143188840625095182 ) ) ;
#2922 = EDGE_CURVE ( 'NONE', #4819, #13956, #3759, .T. ) ;
#2923 = LINE ( 'NONE', #14541, #78 ) ;
#2924 = AXIS2_PLACEMENT_3D ( 'NONE', #5577, #18953, #1934 ) ;
#2925 = EDGE_CURVE ( 'NONE', #11597, #16209, #11437, .T. ) ;
#2926 = VECTOR ( 'NONE', #5481, 1000.000000000000000 ) ;
#2927 = CARTESIAN_POINT ( 'NONE',  ( 53.25483508941461963, -9.531985000000000596, -5.879799058943532941 ) ) ;
#2928 = CARTESIAN_POINT ( 'NONE',  ( 6.714528961867625156, 11.12069169983300299, 2.708914882803345137 ) ) ;
#2929 = DIRECTION ( 'NONE',  ( 0.000000000000000000, 1.000000000000000000, 0.000000000000000000 ) ) ;
#2930 = CARTESIAN_POINT ( 'NONE',  ( 20.17509116920188106, -6.297343119843968218, -15.18573247873388610 ) ) ;
#2931 = CARTESIAN_POINT ( 'NONE',  ( 23.41562500000000213, 0.000000000000000000, 5.159374999999999822 ) ) ;
#2932 = VERTEX_POINT ( 'NONE', #9151 ) ;
#2933 = LINE ( 'NONE', #9660, #12813 ) ;
#2934 = DIRECTION ( 'NONE',  ( 1.000000000000000000, 0.000000000000000000, 0.000000000000000000 ) ) ;
#2935 = CIRCLE ( 'NONE', #817, 3.968750000000000000 ) ;
#2936 = ORIENTED_EDGE ( 'NONE', *, *, #21877, .T. ) ;
#2937 = CARTESIAN_POINT ( 'NONE',  ( 11.91464549116346561, 20.84857631512679177, 3.612794791681625650 ) ) ;
#2938 = LINE ( 'NONE', #6235, #6329 ) ;
#2939 = CARTESIAN_POINT ( 'NONE',  ( 14.41042916532441076, -7.397368266813621140, -15.94011715785100058 ) ) ;
#2940 = CYLINDRICAL_SURFACE ( 'NONE', #15959, 9.524999999999998579 ) ;
#2941 = EDGE_LOOP ( 'NONE', ( #9817, #8604, #12640, #18611 ) ) ;
#2942 = DIRECTION ( 'NONE',  ( 0.000000000000000000, 0.000000000000000000, -1.000000000000000000 ) ) ;
#2943 = VERTEX_POINT ( 'NONE', #13832 ) ;
#2944 = AXIS2_PLACEMENT_3D ( 'NONE', #1782, #12081, #20447 ) ;
#2945 = CARTESIAN_POINT ( 'NONE',  ( 45.06824031473797021, 38.88803500000000213, -7.839138111890849636 ) ) ;
#2946 = CARTESIAN_POINT ( 'NONE',  ( 0.8282372033119331789, 19.59804870509496055, 2.312752627255655113 ) ) ;
#2947 = CARTESIAN_POINT ( 'NONE',  ( 19.65610218525419484, -5.426016033732137700, -14.59150382834396886 ) ) ;
#2948 = ORIENTED_EDGE ( 'NONE', *, *, #16191, .F. ) ;
#2949 = CARTESIAN_POINT ( 'NONE',  ( 9.701140030272853210, 21.05370774754728203, 3.420069439634078279 ) ) ;
#2950 = EDGE_CURVE ( 'NONE', #10465, #1238, #16741, .T. ) ;
#2951 = AXIS2_PLACEMENT_3D ( 'NONE', #11235, #14800, #2510 ) ;
#2952 = DIRECTION ( 'NONE',  ( -0.9579671649362033747, 0.000000000000000000, 0.2868778675745011775 ) ) ;
#2953 = EDGE_CURVE ( 'NONE', #16343, #6924, #2018, .T. ) ;
#2954 = CARTESIAN_POINT ( 'NONE',  ( 7.366404870011150408, 12.62799681450196054, -1.646865681378777646 ) ) ;
#2955 = CARTESIAN_POINT ( 'NONE',  ( 19.16029575344082403, -5.702674460024825365, -15.43937346368577046 ) ) ;
#2956 = FILL_AREA_STYLE ('',( #10012 ) ) ;
#2957 = CIRCLE ( 'NONE', #4723, 1.191259999999999319 ) ;
#2958 = VERTEX_POINT ( 'NONE', #7941 ) ;
#2959 = CARTESIAN_POINT ( 'NONE',  ( 36.54633153140315471, -14.84248999999999974, -9.516661413425623550 ) ) ;
#2960 = DIRECTION ( 'NONE',  ( 0.000000000000000000, 1.000000000000000000, 0.000000000000000000 ) ) ;
#2961 = ORIENTED_EDGE ( 'NONE', *, *, #17403, .T. ) ;
#2962 = ORIENTED_EDGE ( 'NONE', *, *, #11927, .F. ) ;
#2963 = CARTESIAN_POINT ( 'NONE',  ( 20.47011791841445216, -6.007381863893643370, -13.86582502354129254 ) ) ;
#2965 = CYLINDRICAL_SURFACE ( 'NONE', #18054, 1.983740000000001169 ) ;
#2964 = CARTESIAN_POINT ( 'NONE',  ( 0.5847478725274279920, 20.32785531569650317, 1.828616380043220691 ) ) ;
#2966 = ORIENTED_EDGE ( 'NONE', *, *, #19024, .F. ) ;
#2967 = CARTESIAN_POINT ( 'NONE',  ( 3.632615605465845832, 17.33140468479308538, -1.342300317307963509 ) ) ;
#2968 = AXIS2_PLACEMENT_3D ( 'NONE', #8717, #12385, #2308 ) ;
#2969 = ORIENTED_EDGE ( 'NONE', *, *, #8997, .F. ) ;
#2970 = EDGE_LOOP ( 'NONE', ( #17589, #15029, #9937, #142, #13916, #19267 ) ) ;
#2971 = ORIENTED_EDGE ( 'NONE', *, *, #17802, .T. ) ;
#2972 = CARTESIAN_POINT ( 'NONE',  ( 2.232581729494868217, 12.55203364629052665, 2.299247354297082602 ) ) ;
#2973 = AXIS2_PLACEMENT_3D ( 'NONE', #19298, #7264, #12679 ) ;
#2974 = EDGE_CURVE ( 'NONE', #4834, #14162, #12939, .T. ) ;
#2975 = CARTESIAN_POINT ( 'NONE',  ( 4.582301617914484204, 11.87654007454232108, 3.801650534573477458 ) ) ;
#2976 = DIRECTION ( 'NONE',  ( -0.2490110332224855227, 0.000000000000000000, 0.9685006480810791629 ) ) ;
#2977 = CIRCLE ( 'NONE', #18834, 1.190624999999997824 ) ;
#2978 = LINE ( 'NONE', #11254, #7567 ) ;
#2979 = DIRECTION ( 'NONE',  ( 0.2490110332224850231, 0.000000000000000000, -0.9685006480810791629 ) ) ;
#2980 = DIRECTION ( 'NONE',  ( 0.05085730733808393328, 0.000000000000000000, -0.9987059298363656357 ) ) ;
#2981 = CARTESIAN_POINT ( 'NONE',  ( 3.634673347361986551, 15.97827594584995481, 9.198068844196187754 ) ) ;
#2982 = ORIENTED_EDGE ( 'NONE', *, *, #5220, .F. ) ;
#2983 = CYLINDRICAL_SURFACE ( 'NONE', #7522, 0.7950200000000001710 ) ;
#2984 = CARTESIAN_POINT ( 'NONE',  ( -16.07247711516169275, -5.309201820043501385, -10.44681224123558039 ) ) ;
#2985 = DIRECTION ( 'NONE',  ( 0.000000000000000000, 1.000000000000000000, 0.000000000000000000 ) ) ;
#2986 = DIRECTION ( 'NONE',  ( 0.000000000000000000, 1.000000000000000000, 0.000000000000000000 ) ) ;
#2987 = CARTESIAN_POINT ( 'NONE',  ( 56.91751438644678984, 0.000000000000000000, -20.96198986413465448 ) ) ;
#2988 = ORIENTED_EDGE ( 'NONE', *, *, #8997, .T. ) ;
#2989 = ORIENTED_EDGE ( 'NONE', *, *, #3460, .F. ) ;
#2990 = CARTESIAN_POINT ( 'NONE',  ( 10.81515204167621924, 18.24951553479433031, -3.654582590115240226 ) ) ;
#2991 = DIRECTION ( 'NONE',  ( 0.000000000000000000, 1.000000000000000000, 0.000000000000000000 ) ) ;
#2992 = CIRCLE ( 'NONE', #15356, 0.5079999999999976756 ) ;
#2993 = CARTESIAN_POINT ( 'NONE',  ( 11.15957945745538815, 12.36081089520519605, -2.843515111212955748 ) ) ;
#2994 = VERTEX_POINT ( 'NONE', #6273 ) ;
#2995 = EDGE_LOOP ( 'NONE', ( #11838, #1015 ) ) ;
#2996 = CYLINDRICAL_SURFACE ( 'NONE', #1774, 0.3962399999999990929 ) ;
#2997 = CARTESIAN_POINT ( 'NONE',  ( 8.885977996197350848, 12.18137409406300620, 4.901112392138662344 ) ) ;
#2998 = VECTOR ( 'NONE', #2533, 1000.000000000000227 ) ;
#2999 = ADVANCED_FACE ( 'NONE', ( #11044 ), #2646, .T. ) ;
#3000 = DIRECTION ( 'NONE',  ( 0.000000000000000000, -1.000000000000000000, 0.000000000000000000 ) ) ;
#3001 = CARTESIAN_POINT ( 'NONE',  ( 3.360635606688116894, -3.968114999999999615, -20.45316710734507026 ) ) ;
#3002 = CARTESIAN_POINT ( 'NONE',  ( 2.855389239292441150, 11.23804227924006227, 5.233798368148996794 ) ) ;
#3003 = CARTESIAN_POINT ( 'NONE',  ( 0.7890252754738890095, 11.42114643257019146, 4.969940827006558592 ) ) ;
#3004 = DIRECTION ( 'NONE',  ( -0.2868778675745011220, 0.000000000000000000, -0.9579671649362033747 ) ) ;
#3005 = VERTEX_POINT ( 'NONE', #17899 ) ;
#3006 = CARTESIAN_POINT ( 'NONE',  ( 3.448768254860767435, 13.61749910441900191, 7.578225799708883770 ) ) ;
#3007 = DIRECTION ( 'NONE',  ( -0.9767031480033347979, 0.000000000000000000, 0.2145948757085687775 ) ) ;
#3008 = DIRECTION ( 'NONE',  ( -0.9685006480810794960, 0.000000000000000000, -0.2490110332224836354 ) ) ;
#3009 = CARTESIAN_POINT ( 'NONE',  ( 9.114141643690045314, 30.63641399982339308, -21.02279864880779670 ) ) ;
#3010 = AXIS2_PLACEMENT_3D ( 'NONE', #11862, #6884, #17164 ) ;
#3011 = FACE_OUTER_BOUND ( 'NONE', #16940, .T. ) ;
#3012 = ORIENTED_EDGE ( 'NONE', *, *, #478, .T. ) ;
#3013 = DIRECTION ( 'NONE',  ( 0.9964481331860212121, 0.000000000000000000, -0.08420877549337300871 ) ) ;
#3014 = CARTESIAN_POINT ( 'NONE',  ( 7.462231758176627316, 21.81816933872264030, 3.277137776123120183 ) ) ;
#3015 = CARTESIAN_POINT ( 'NONE',  ( 9.166816848515864535, 13.36017816153255211, -2.795096715123733588 ) ) ;
#3016 = ORIENTED_EDGE ( 'NONE', *, *, #3725, .T. ) ;
#3017 = CARTESIAN_POINT ( 'NONE',  ( 8.855399128654450891, 19.86079412954436663, 6.740554311246585328 ) ) ;
#3018 = DIRECTION ( 'NONE',  ( -0.6702301885068630005, 0.000000000000000000, -0.7421532822901579785 ) ) ;
#3019 = CARTESIAN_POINT ( 'NONE',  ( 3.416691995540810822, 16.48226916726223479, 8.524304092238224939 ) ) ;
#3020 = EDGE_CURVE ( 'NONE', #3845, #9830, #9375, .T. ) ;
#3021 = CARTESIAN_POINT ( 'NONE',  ( 49.41195815393805901, 42.06303499999999929, -1.411525001868561224 ) ) ;
#3022 = CARTESIAN_POINT ( 'NONE',  ( 6.665396026729170309, 19.45118757208885896, 6.417806572678339094 ) ) ;
#3023 = DIRECTION ( 'NONE',  ( 0.9173788132826626862, 0.000000000000000000, -0.3980152169705242216 ) ) ;
#3024 = AXIS2_PLACEMENT_3D ( 'NONE', #18003, #11482, #7943 ) ;
#3025 = ADVANCED_FACE ( 'NONE', ( #21418 ), #19430, .F. ) ;
#3026 = EDGE_CURVE ( 'NONE', #1402, #6719, #19648, .T. ) ;
#3027 = CARTESIAN_POINT ( 'NONE',  ( 12.09589873078120270, 11.13638386089868249, 0.7328227269680089861 ) ) ;
#3028 = EDGE_CURVE ( 'NONE', #7335, #17408, #19956, .T. ) ;
#3029 = CARTESIAN_POINT ( 'NONE',  ( 3.094989319135907913, 19.78346126529704208, 7.974999081070190066 ) ) ;
#3030 = DIRECTION ( 'NONE',  ( 0.08420877549337300871, 0.000000000000000000, 0.9964481331860212121 ) ) ;
#3031 = PLANE ( 'NONE',  #17410 ) ;
#3032 = CARTESIAN_POINT ( 'NONE',  ( 53.92979111630407374, -6.356984999999459873, -15.65141968182990162 ) ) ;
#3033 = CYLINDRICAL_SURFACE ( 'NONE', #2674, 1.190624999999999378 ) ;
#3034 = CARTESIAN_POINT ( 'NONE',  ( 21.19398735712951876, -3.814682859859762853, -15.02299825110072895 ) ) ;
#3035 = CYLINDRICAL_SURFACE ( 'NONE', #21566, 3.175000000000001155 ) ;
#3036 = ORIENTED_EDGE ( 'NONE', *, *, #14919, .F. ) ;
#3037 = DIRECTION ( 'NONE',  ( 0.3447671952293626108, 0.000000000000000000, 0.9386882235831439658 ) ) ;
#3038 = FACE_OUTER_BOUND ( 'NONE', #10072, .T. ) ;
#3039 = ORIENTED_EDGE ( 'NONE', *, *, #13022, .F. ) ;
#3040 = CARTESIAN_POINT ( 'NONE',  ( 11.86489017329819085, 20.90669377702615250, 3.480282917028821199 ) ) ;
#3041 = CARTESIAN_POINT ( 'NONE',  ( 52.76334005444670794, 38.88803500000000213, -23.57731578991186083 ) ) ;
#3042 = CYLINDRICAL_SURFACE ( 'NONE', #2575, 3.968750000000001776 ) ;
#3043 = CARTESIAN_POINT ( 'NONE',  ( 16.95410740259722004, 1.821792332331595432, -14.48457991158913494 ) ) ;
#3045 = DIRECTION ( 'NONE',  ( -0.6702301885068630005, 0.000000000000000000, -0.7421532822901579785 ) ) ;
#3044 = CARTESIAN_POINT ( 'NONE',  ( 6.279877271179575615, 11.31448603738602188, 4.296343679347063294 ) ) ;
#3046 = ORIENTED_EDGE ( 'NONE', *, *, #2107, .F. ) ;
#3047 = CARTESIAN_POINT ( 'NONE',  ( 0.000000000000000000, 0.000000000000000000, 0.000000000000000000 ) ) ;
#3048 = EDGE_CURVE ( 'NONE', #12509, #19832, #7231, .T. ) ;
#3049 = CARTESIAN_POINT ( 'NONE',  ( 46.03750000000000142, -9.531985000000000596, -10.31874999999999964 ) ) ;
#3050 = CARTESIAN_POINT ( 'NONE',  ( 3.843255135554278556, 17.07327212836336372, -0.6144225183285193514 ) ) ;
#3051 = ORIENTED_EDGE ( 'NONE', *, *, #843, .F. ) ;
#3052 = CARTESIAN_POINT ( 'NONE',  ( 19.52483535838462814, -0.1223081128681305918, -14.99489796488201421 ) ) ;
#3053 = ORIENTED_EDGE ( 'NONE', *, *, #15516, .F. ) ;
#3054 = CARTESIAN_POINT ( 'NONE',  ( 5.535879021512672082, 15.56565457311297251, -1.414609335357769559 ) ) ;
#3055 = EDGE_CURVE ( 'NONE', #14160, #18035, #18119, .T. ) ;
#3056 = CARTESIAN_POINT ( 'NONE',  ( 38.22597429223493748, 39.04395605175655248, -4.868457244536984696 ) ) ;
#3057 = CARTESIAN_POINT ( 'NONE',  ( 5.391407144478529645, 13.59023913265000338, -1.534842905340066954 ) ) ;
#3058 = CARTESIAN_POINT ( 'NONE',  ( -6.268352501591477832, 33.32892749999999893, -35.49402737582407497 ) ) ;
#3059 = DIRECTION ( 'NONE',  ( -0.4128958666089267981, 0.5884034904305870395, 0.6951966166390379787 ) ) ;
#3060 = ORIENTED_EDGE ( 'NONE', *, *, #21551, .T. ) ;
#3061 = CARTESIAN_POINT ( 'NONE',  ( 10.88042432497300638, 18.51148264076616101, 6.327082982554776081 ) ) ;
#3062 = CARTESIAN_POINT ( 'NONE',  ( 7.229729504486647862, 14.38111527192631200, -2.659786112516965062 ) ) ;
#3063 = LINE ( 'NONE', #1181, #3943 ) ;
#3064 = VERTEX_POINT ( 'NONE', #7616 ) ;
#3065 = ORIENTED_EDGE ( 'NONE', *, *, #10197, .T. ) ;
#3066 = CARTESIAN_POINT ( 'NONE',  ( -22.90765545213488963, 39.44874000000000080, -9.869178565316103047 ) ) ;
#3068 = CARTESIAN_POINT ( 'NONE',  ( 46.03750000000000142, -1.983739999999999837, -10.31874999999999964 ) ) ;
#3067 = CARTESIAN_POINT ( 'NONE',  ( 3.342050458355601883, 21.45407066062478307, 3.539861934473672811 ) ) ;
#3069 = ORIENTED_EDGE ( 'NONE', *, *, #6085, .T. ) ;
#3070 = CARTESIAN_POINT ( 'NONE',  ( 5.639002058890934421, 21.52895174503652953, 3.779455238249453064 ) ) ;
#3071 = EDGE_CURVE ( 'NONE', #8830, #13930, #2978, .T. ) ;
#3072 = ORIENTED_EDGE ( 'NONE', *, *, #12490, .F. ) ;
#3073 = ADVANCED_FACE ( 'NONE', ( #970 ), #16468, .F. ) ;
#3074 = ADVANCED_FACE ( 'NONE', ( #2747 ), #6388, .F. ) ;
#3075 = ORIENTED_EDGE ( 'NONE', *, *, #7315, .F. ) ;
#3076 = CARTESIAN_POINT ( 'NONE',  ( 1.120844084417135011, 12.59384379629693207, 6.529727573272420038 ) ) ;
#3077 = CARTESIAN_POINT ( 'NONE',  ( 46.03750000000000142, 0.000000000000000000, -10.31874999999999964 ) ) ;
#3078 = ORIENTED_EDGE ( 'NONE', *, *, #2543, .T. ) ;
#3079 = CARTESIAN_POINT ( 'NONE',  ( 2.525842802073233084, 12.09107524552456603, 3.660819305400447199 ) ) ;
#3080 = CARTESIAN_POINT ( 'NONE',  ( 9.612433970843095921, 14.64457645186116252, 7.826711049808183773 ) ) ;
#3081 = DIRECTION ( 'NONE',  ( 0.000000000000000000, 1.000000000000000000, 0.000000000000000000 ) ) ;
#3082 = CARTESIAN_POINT ( 'NONE',  ( 32.42378190387104553, 34.52875999999999834, -18.15178106273469183 ) ) ;
#3083 = LINE ( 'NONE', #6390, #13266 ) ;
#3084 = CARTESIAN_POINT ( 'NONE',  ( 2.013765651847553073, 18.70393287884557054, -0.1586800916523363469 ) ) ;
#3085 = EDGE_LOOP ( 'NONE', ( #12373, #15790, #10238, #21050 ) ) ;
#3086 = CYLINDRICAL_SURFACE ( 'NONE', #19163, 0.5080000000000023386 ) ;
#3087 = CARTESIAN_POINT ( 'NONE',  ( 32.17043356788648367, 32.54502000000000095, -17.71146456218788146 ) ) ;
#3088 = CARTESIAN_POINT ( 'NONE',  ( 1.998220421679061776, -1.515722362770699494, -22.64748046904500356 ) ) ;
#3089 = CARTESIAN_POINT ( 'NONE',  ( 53.83137747314165722, 38.57687151959435568, -15.79457933408115089 ) ) ;
#3090 = ORIENTED_EDGE ( 'NONE', *, *, #5055, .F. ) ;
#3091 = VERTEX_POINT ( 'NONE', #19551 ) ;
#3092 = CARTESIAN_POINT ( 'NONE',  ( 11.63887962177664015, 21.02863807409008245, 3.776004642387295274 ) ) ;
#3093 = CIRCLE ( 'NONE', #15100, 5.357812499999999645 ) ;
#3094 = DIRECTION ( 'NONE',  ( -0.9987059298363657467, 0.000000000000000000, -0.05085730733808409287 ) ) ;
#3095 = VERTEX_POINT ( 'NONE', #4418 ) ;
#3096 = ORIENTED_EDGE ( 'NONE', *, *, #21078, .F. ) ;
#3097 = EDGE_CURVE ( 'NONE', #17763, #15906, #13157, .T. ) ;
#3098 = PLANE ( 'NONE',  #8140 ) ;
#3099 = CARTESIAN_POINT ( 'NONE',  ( 8.105578319609293203, 11.67745808062331214, 1.442659932574160253 ) ) ;
#3100 = AXIS2_PLACEMENT_3D ( 'NONE', #4172, #6039, #14259 ) ;
#3101 = FACE_BOUND ( 'NONE', #14158, .T. ) ;
#3102 = CARTESIAN_POINT ( 'NONE',  ( 13.62051399351888747, 17.23237496650334677, -17.80340391586448234 ) ) ;
#3103 = CARTESIAN_POINT ( 'NONE',  ( -0.1543974142126335047, 14.11522100541123592, 0.5695158722648775429 ) ) ;
#3104 = CARTESIAN_POINT ( 'NONE',  ( -51.84779601320726528, -5.714999999999999858, -70.46818750274715626 ) ) ;
#3105 = ORIENTED_EDGE ( 'NONE', *, *, #10351, .F. ) ;
#3106 = CARTESIAN_POINT ( 'NONE',  ( 0.8541095398342212208, 12.13066582883064193, 4.831952372105788207 ) ) ;
#3107 = LINE ( 'NONE', #16714, #19112 ) ;
#3108 = CARTESIAN_POINT ( 'NONE',  ( 29.76562500000000000, 30.56064500000000095, -4.317999999999999616 ) ) ;
#3109 = CARTESIAN_POINT ( 'NONE',  ( 12.88896270848683123, -7.596525905234238429, -15.53747963948190325 ) ) ;
#3110 = DIRECTION ( 'NONE',  ( 0.000000000000000000, 1.000000000000000000, 0.000000000000000000 ) ) ;
#3111 = VERTEX_POINT ( 'NONE', #7826 ) ;
#3112 = CARTESIAN_POINT ( 'NONE',  ( 9.377360826946816275, 19.33115936737788232, -2.952836903115966471 ) ) ;
#3113 = CARTESIAN_POINT ( 'NONE',  ( 37.35186600153178915, 38.88803500000000213, -2.356229033655170113 ) ) ;
#3114 = CARTESIAN_POINT ( 'NONE',  ( 9.199613818395116382, 17.51864436858641838, -3.513625226794980350 ) ) ;
#3115 = VERTEX_POINT ( 'NONE', #4189 ) ;
#3116 = EDGE_CURVE ( 'NONE', #7624, #6616, #2858, .T. ) ;
#3117 = VECTOR ( 'NONE', #17381, 1000.000000000000000 ) ;
#3118 = CARTESIAN_POINT ( 'NONE',  ( 6.992329041007389279, 21.55996507129514939, 1.710843802307564721 ) ) ;
#3119 = CARTESIAN_POINT ( 'NONE',  ( 7.735533989518945219, 5.548947500000001476, -21.17236077523805449 ) ) ;
#3120 = CARTESIAN_POINT ( 'NONE',  ( 3.471600356522836606, 14.96929529427155714, 8.313123240795297519 ) ) ;
#3121 = DIRECTION ( 'NONE',  ( 0.000000000000000000, 0.000000000000000000, 1.000000000000000000 ) ) ;
#3122 = DIRECTION ( 'NONE',  ( 0.000000000000000000, -1.000000000000000000, 0.000000000000000000 ) ) ;
#3123 = PLANE ( 'NONE',  #7204 ) ;
#3124 = EDGE_LOOP ( 'NONE', ( #11928, #5178, #8186, #2072 ) ) ;
#3125 = CARTESIAN_POINT ( 'NONE',  ( 32.18388890846549799, 34.52875999999999834, 1.507793899792891468 ) ) ;
#3126 = CARTESIAN_POINT ( 'NONE',  ( 11.40763102503163218, 14.41047425500502754, -3.504232829823089368 ) ) ;
#3127 = CARTESIAN_POINT ( 'NONE',  ( 3.352276079298180722, 11.89587513260652152, 6.861475299447377552 ) ) ;
#3128 = DIRECTION ( 'NONE',  ( 0.9964481331860213231, 0.000000000000000000, -0.08420877549337293932 ) ) ;
#3129 = LINE ( 'NONE', #11636, #5032 ) ;
#3130 = CARTESIAN_POINT ( 'NONE',  ( 6.396056618077795797, 11.71523274630726164, 2.847703469759983008 ) ) ;
#3131 = DIRECTION ( 'NONE',  ( -1.000000000000000000, 0.000000000000000000, 0.000000000000000000 ) ) ;
#3132 = EDGE_CURVE ( 'NONE', #9903, #5598, #9324, .T. ) ;
#3133 = DIRECTION ( 'NONE',  ( 0.2868778675745011220, 0.000000000000000000, 0.9579671649362033747 ) ) ;
#3134 = CARTESIAN_POINT ( 'NONE',  ( 30.41963056417667488, 32.54502000000000095, -8.653862521447852174 ) ) ;
#3135 = ORIENTED_EDGE ( 'NONE', *, *, #2620, .F. ) ;
#3136 = LINE ( 'NONE', #16630, #17400 ) ;
#3137 = DIRECTION ( 'NONE',  ( -0.3928209820863007296, 0.000000000000000000, 0.9196149607486571176 ) ) ;
#3138 = VECTOR ( 'NONE', #10654, 1000.000000000000000 ) ;
#3139 = ORIENTED_EDGE ( 'NONE', *, *, #11678, .F. ) ;
#3140 = EDGE_CURVE ( 'NONE', #5733, #17811, #3343, .T. ) ;
#3141 = CARTESIAN_POINT ( 'NONE',  ( 12.85889632468635568, 18.41644950543497572, 5.976846945769059616 ) ) ;
#3142 = CARTESIAN_POINT ( 'NONE',  ( 46.03750000000000142, -9.531985000000000596, -10.31874999999999964 ) ) ;
#3143 = EDGE_CURVE ( 'NONE', #16035, #7874, #18138, .T. ) ;
#3144 = CARTESIAN_POINT ( 'NONE',  ( 14.22429864969880065, 1.227399424245292137, -15.50635713965766982 ) ) ;
#3146 = CARTESIAN_POINT ( 'NONE',  ( 17.22522857595987844, -1.983739999999999393, -15.04442098945225403 ) ) ;
#3145 = CARTESIAN_POINT ( 'NONE',  ( 6.985997644112802440, 16.61588919119046182, 8.232423580698503329 ) ) ;
#3147 = ORIENTED_EDGE ( 'NONE', *, *, #21018, .T. ) ;
#3148 = CARTESIAN_POINT ( 'NONE',  ( -14.99341658050624027, -4.186290746340128877, -10.07873794320046912 ) ) ;
#3149 = LINE ( 'NONE', #21492, #8411 ) ;
#3150 = ORIENTED_EDGE ( 'NONE', *, *, #11028, .T. ) ;
#3151 = DIRECTION ( 'NONE',  ( -1.000000000000000000, 0.000000000000000000, 0.000000000000000000 ) ) ;
#3152 = ORIENTED_EDGE ( 'NONE', *, *, #21472, .T. ) ;
#3153 = CARTESIAN_POINT ( 'NONE',  ( 9.216504298751090118, 16.57988186816537279, 7.325230060800960175 ) ) ;
#3154 = DIRECTION ( 'NONE',  ( -0.9579671649362032637, 0.000000000000000000, 0.2868778675745010664 ) ) ;
#3155 = CARTESIAN_POINT ( 'NONE',  ( 11.10672801841564628, 12.31819272753022254, -2.965602515288232155 ) ) ;
#3156 = EDGE_CURVE ( 'NONE', #21599, #17693, #18225, .T. ) ;
#3157 = CARTESIAN_POINT ( 'NONE',  ( 16.37115362237207705, -7.227104028295391558, -16.00107671334114556 ) ) ;
#3158 = LINE ( 'NONE', #15016, #5901 ) ;
#3159 = ORIENTED_EDGE ( 'NONE', *, *, #14297, .F. ) ;
#3160 = CARTESIAN_POINT ( 'NONE',  ( 9.140504733104041435, 21.05562268498557188, 1.832113029465568754 ) ) ;
#3161 = CARTESIAN_POINT ( 'NONE',  ( 6.292329232406544293, 20.69394519596638204, -0.2665356535715593389 ) ) ;
#3162 = CARTESIAN_POINT ( 'NONE',  ( 8.776506035771831193, 2.891917824018316097, -16.46252061043899673 ) ) ;
#3163 = EDGE_LOOP ( 'NONE', ( #18876, #2795, #11472, #13590 ) ) ;
#3164 = ORIENTED_EDGE ( 'NONE', *, *, #5578, .T. ) ;
#3165 = LINE ( 'NONE', #9897, #2805 ) ;
#3166 = EDGE_CURVE ( 'NONE', #3464, #7494, #8611, .T. ) ;
#3168 = LINE ( 'NONE', #16348, #14535 ) ;
#3167 = CARTESIAN_POINT ( 'NONE',  ( 1.548022356803757216, 14.62510310756713672, -0.4782326917522521370 ) ) ;
#3169 = VERTEX_POINT ( 'NONE', #8888 ) ;
#3170 = CARTESIAN_POINT ( 'NONE',  ( 6.850747683931677656, 19.94702954872458989, 7.017284919865954151 ) ) ;
#3171 = VECTOR ( 'NONE', #4795, 1000.000000000000000 ) ;
#3172 = ORIENTED_EDGE ( 'NONE', *, *, #5270, .T. ) ;
#3173 = VERTEX_POINT ( 'NONE', #17080 ) ;
#3174 = ADVANCED_FACE ( 'NONE', ( #15038 ), #16574, .F. ) ;
#3175 = VECTOR ( 'NONE', #9870, 1000.000000000000000 ) ;
#3176 = CARTESIAN_POINT ( 'NONE',  ( -51.02421882195815783, -5.714364999999999029, -23.02637480153789795 ) ) ;
#3177 = ORIENTED_EDGE ( 'NONE', *, *, #3301, .T. ) ;
#3178 = CARTESIAN_POINT ( 'NONE',  ( 6.355167927674128414, 20.69792818844234361, -0.2884820177363571769 ) ) ;
#3179 = CARTESIAN_POINT ( 'NONE',  ( 3.964049121815345966, 12.88683406160677158, 0.9507199798804107926 ) ) ;
#3180 = AXIS2_PLACEMENT_3D ( 'NONE', #19584, #21237, #19469 ) ;
#3181 = CARTESIAN_POINT ( 'NONE',  ( 24.36723594150488026, 30.55334249999999940, 1.799757394719970982 ) ) ;
#3182 = ADVANCED_FACE ( 'NONE', ( #11587 ), #7010, .T. ) ;
#3183 = VECTOR ( 'NONE', #48, 1000.000000000000000 ) ;
#3184 = CARTESIAN_POINT ( 'NONE',  ( 53.11257091495114935, -7.547610000000002373, -16.69598124282935458 ) ) ;
#3185 = CARTESIAN_POINT ( 'NONE',  ( 1.864081481279129537, 12.78457889254149649, 0.7313840301176890435 ) ) ;
#3186 = ADVANCED_FACE ( 'NONE', ( #6508 ), #13269, .T. ) ;
#3187 = VECTOR ( 'NONE', #10703, 1000.000000000000000 ) ;
#3188 = EDGE_CURVE ( 'NONE', #6627, #5674, #16681, .T. ) ;
#3189 = VERTEX_POINT ( 'NONE', #8266 ) ;
#3190 = CARTESIAN_POINT ( 'NONE',  ( -17.46249999999999858, 1.984375000000000000, 0.000000000000000000 ) ) ;
#3191 = LINE ( 'NONE', #13477, #9964 ) ;
#3192 = CARTESIAN_POINT ( 'NONE',  ( 13.15380310827069010, 21.44506156727471335, 1.916236206408076903 ) ) ;
#3193 = CARTESIAN_POINT ( 'NONE',  ( 19.78100715883822147, -2.554695793581883478, -14.20785545507690095 ) ) ;
#3194 = ORIENTED_EDGE ( 'NONE', *, *, #19561, .F. ) ;
#3195 = ORIENTED_EDGE ( 'NONE', *, *, #15367, .T. ) ;
#3196 = CARTESIAN_POINT ( 'NONE',  ( 7.747576815138661921, 12.05201058041374118, 0.2846308798510710503 ) ) ;
#3197 = AXIS2_PLACEMENT_3D ( 'NONE', #2911, #5104, #6758 ) ;
#3198 = DIRECTION ( 'NONE',  ( -0.2490110332224849676, 0.000000000000000000, 0.9685006480810792739 ) ) ;
#3199 = ORIENTED_EDGE ( 'NONE', *, *, #5708, .T. ) ;
#3200 = ORIENTED_EDGE ( 'NONE', *, *, #13479, .F. ) ;
#3201 = DIRECTION ( 'NONE',  ( 0.2868778675745010664, 0.000000000000000000, 0.9579671649362032637 ) ) ;
#3202 = ORIENTED_EDGE ( 'NONE', *, *, #11727, .F. ) ;
#3203 = CIRCLE ( 'NONE', #16238, 5.357812499999999645 ) ;
#3204 = CARTESIAN_POINT ( 'NONE',  ( 9.270728378017370375, 14.93585744516916236, 7.021239391598488311 ) ) ;
#3205 = VECTOR ( 'NONE', #21069, 1000.000000000000000 ) ;
#3206 = DIRECTION ( 'NONE',  ( -0.2490110332224850509, 0.000000000000000000, 0.9685006480810792739 ) ) ;
#3207 = AXIS2_PLACEMENT_3D ( 'NONE', #5858, #16163, #5960 ) ;
#3208 = AXIS2_PLACEMENT_3D ( 'NONE', #6263, #10022, #6493 ) ;
#3209 = DIRECTION ( 'NONE',  ( 0.05085730733808393328, 0.000000000000000000, -0.9987059298363656357 ) ) ;
#3210 = CARTESIAN_POINT ( 'NONE',  ( 3.454954327428137351, 15.44872671029758671, -1.443864749231975830 ) ) ;
#3211 = CARTESIAN_POINT ( 'NONE',  ( -0.1786810500680980907, 15.98335145267441249, 0.04971173333621729806 ) ) ;
#3212 = EDGE_CURVE ( 'NONE', #20891, #12179, #162, .T. ) ;
#3213 = DIRECTION ( 'NONE',  ( 0.000000000000000000, -1.000000000000000000, -0.000000000000000000 ) ) ;
#3214 = ORIENTED_EDGE ( 'NONE', *, *, #7590, .F. ) ;
#3215 = CARTESIAN_POINT ( 'NONE',  ( 0.4780110449530477479, 13.07040487695864250, 2.031854558472322658 ) ) ;
#3216 = CARTESIAN_POINT ( 'NONE',  ( 42.94469661997857912, -9.531985000000000596, -18.48251861828712705 ) ) ;
#3217 = DIRECTION ( 'NONE',  ( 0.000000000000000000, -1.000000000000000000, 0.000000000000000000 ) ) ;
#3218 = LINE ( 'NONE', #6862, #12803 ) ;
#3219 = AXIS2_PLACEMENT_3D ( 'NONE', #4230, #21031, #16082 ) ;
#3220 = DIRECTION ( 'NONE',  ( 0.9579671649362032637, 0.000000000000000000, -0.2868778675745011775 ) ) ;
#3221 = ORIENTED_EDGE ( 'NONE', *, *, #17405, .T. ) ;
#3222 = CARTESIAN_POINT ( 'NONE',  ( 6.788691988670617405, 21.59576476661624156, 1.422531602670973561 ) ) ;
#3223 = CYLINDRICAL_SURFACE ( 'NONE', #11355, 3.174999999999999822 ) ;
#3224 = B_SPLINE_CURVE_WITH_KNOTS ( 'NONE', 3,
 ( #1590, #13228, #8332, #6668, #11544, #17614, #14319, #14100, #20803, #5989, #5671, #2468, #21039, #14422, #5884, #2792, #7661, #12875, #19370, #2580, #2356, #2691, #4351, #7556, #10768, #4125, #11092, #17732, #9196, #4236, #1018, #16086, #16193, #9087, #10976, #15980, #811, #15864, #19158, #12760, #16296, #12430, #693, #4024, #10868, #9420, #9312, #17511, #14213, #7438, #21250, #916, #17845, #19481, #7765, #20927, #21135, #14532, #4460, #6103, #19594, #5787, #11192, #17944, #9528, #12546, #19270, #10076, #14974, #6640, #13404, #1130, #20114, #18361, #18050, #6211, #8199, #1341, #4987, #8305, #8083, #16723, #18475, #6434, #21689, #11743, #21460, #3118, #14858, #18166, #7983, #12982, #14754, #3344, #9638, #1565, #9965, #20010, #16404, #3229, #21354, #1240, #7871, #19913, #19691, #9742, #16612, #14648, #9842, #4560, #11303, #13090, #2907, #21573, #4784, #6317, #19800, #11514, #4675, #11418, #3017, #16505, #13201, #6547, #18257, #1452, #13308, #4880, #11626, #15077, #21790, #461, #8632, #12069, #11849, #17258, #15510, #13855, #1993, #18907, #13520, #5304, #5202, #230, #10512, #3665, #3778, #18580, #13740, #11952, #3551, #3443, #6755, #340, #3888, #12288, #16922, #6871, #18683, #2099, #10178, #20228, #1769, #5101, #8845, #18795, #20556, #7085, #15624, #8516, #10289, #10411, #13972, #7210, #5418, #17038, #1885, #15408, #20669, #20434, #5529, #16821, #8734, #19013, #1663, #8401, #15177, #12183, #15296, #6, #121, #6970, #13630, #20328, #17153, #6078, #2220, #14294, #2666, #9169, #11064, #12619, #2444, #5762, #17487, #566, #2330, #7742, #19130, #17820, #19451, #7635, #3998, #12727, #8961, #10946, #15738, #4210, #19342, #9395, #4326, #12519, #15952, #14502, #668, #7310, #21219, #9285, #14187, #12850, #16164, #14397, #893, #783, #9064, #15839, #21014, #5962, #21110, #10843, #14074, #20781, #19242, #19571, #17702, #20895, #990, #10626, #5860, #17379, #2554, #5643, #7413, #4104, #12404, #10741, #17591, #7531, #16061, #4439, #9503, #2767, #16274, #7849, #1105, #14624, #21333, #11169, #17920, #6193, #12960, #11870, #16841, #13758, #13991, #20690, #3684, #20246, #13881, #13648, #15423, #10532, #8421, #18595, #8650, #249, #3465, #15198, #17278, #5547, #20578, #20348, #140, #5120, #10094, #12202, #1682, #18925, #12306, #6989, #17169, #1794, #5329, #17056, #5217, #10199, #25, #16942, #479, #8536, #3796, #2124, #359, #15315, #5439, #6775, #10427, #13539, #18817, #12094, #8865, #15652, #11976, #1902, #7233, #6887, #18706, #3365, #2009, #3574, #10314, #20459, #8749, #15530, #7111, #1014, #9417, #9082, #7761, #10864, #15975, #7329, #7654, #16083, #17842, #7433, #4122, #19033, #3907, #17726, #10649, #14208, #17610, #4232, #14417, #20923, #9191, #807, #12425, #6100, #10971, #7552, #5666, #2242, #11087, #14527, #21132, #5782, #15858, #14094, #17401, #5984, #8980, #12754, #21245, #2464, #2576, #15758, #17507, #21032, #14315, #20799, #19476, #5881, #585, #4017, #12643, #19367, #19154, #4347, #10764, #2687, #2352, #688, #12540, #9308, #19266, #16185, #913, #7978, #4672, #21788, #14969, #19793, #2786, #1338, #4782, #16722, #3015, #1559, #6314, #7868, #11295, #13088, #16292, #13306, #4457, #8081, #1125, #1448, #9840, #6207, #9962, #21685, #14644, #11416, #14750, #14855, #19910, #12870, #9523, #6545, #16609, #3114, #18162, #19686, #18045, #21570, #8196, #20008, #9740, #4878, #21349, #16502, #8303, #13199, #1237, #11623, #19590, #6429, #15075, #11512, #11188, #2902, #9635, #18358, #3225, #17940, #12978, #4556, #16400, #18255, #8398, #10176, #10283, #13626, #5098, #18790, #2095, #12178, #18902, #15617, #15174, #20110, #17033, #17253, #8840, #6966, #1661, #3546, #4, #3774, #1989, #6750, #11740, #13732, #6867, #10509, #13848, #20324, #6637, #4983, #1880, #20551, #5195, #7080, #13517, #16919, #20226, #11847, #8730, #18575, #13401, #3441, #5414, #15506, #3660, #1765, #334, #18473, #20430, #3341, #226, #15404, #10071, #16819, #8511, #15291, #5300, #118, #11948, #18677, #12063, #8627, #10404, #17149, #15948, #9391, #9164, #4320, #12723, #12399, #11060, #14183, #19237, #13966, #5638, #10839, #5524, #15733, #19446, #456, #7206, #21008, #20665, #10737, #20888, #7527, #5758, #17816, #776, #5957, #12514, #17587, #17371, #888, #5855, #19338, #14290, #2548, #19008, #2439, #17482, #4100, #16057, #12615, #9281, #2215, #4205, #2326, #9060, #8957, #12284, #10942, #3884, #2661, #562, #19123, #15835, #7629, #7306, #10622, #14069, #20776, #14392, #17697, #21106, #3993, #662, #7409, #2877, #2993, #13570, #18527, #13459, #9608, #1214, #7956, #20274, #19767, #1718, #9497, #21434, #11897, #7737, #4642, #8455, #14727, #16871, #16270, #4531, #2762, #17916, #3392, #9717, #21215, #1100, #6287, #11388, #18626, #10126, #15228, #14498, #16481, #6073, #1316, #8059, #59, #6809, #5145, #11794, #14830, #3493, #16159, #18134, #12845, #21543, #6697, #985, #20169, #19567, #5044, #4434, #11165, #6188, #7843, #14620, #21328, #12956, #19664, #11270, #18018, #16375, #7357, #19062, #20378, #3717, #12124, #20610, #17306, #10228, #8780, #5698, #10561, #15785, #2035, #5468 ),
 .UNSPECIFIED., .F., .F.,
 ( 4, 3, 3, 3, 3, 3, 3, 3, 3, 3, 3, 3, 3, 3, 3, 3, 3, 3, 3, 3, 3, 3, 3, 3, 3, 3, 3, 3, 3, 3, 3, 3, 3, 3, 3, 3, 3, 3, 3, 3, 3, 3, 3, 3, 3, 3, 3, 3, 3, 3, 3, 3, 3, 3, 3, 3, 3, 3, 3, 3, 3, 3, 3, 3, 3, 3, 3, 3, 3, 3, 3, 3, 3, 3, 3, 3, 3, 3, 3, 3, 3, 3, 3, 3, 3, 3, 3, 3, 3, 3, 3, 3, 3, 3, 3, 3, 3, 3, 3, 3, 3, 3, 3, 3, 3, 3, 3, 3, 3, 3, 3, 3, 3, 3, 3, 3, 3, 3, 3, 3, 3, 3, 3, 3, 3, 3, 3, 3, 3, 3, 3, 3, 3, 3, 3, 3, 3, 3, 3, 3, 3, 3, 3, 3, 3, 3, 3, 3, 3, 3, 3, 3, 3, 3, 3, 3, 3, 3, 3, 3, 3, 3, 3, 3, 3, 3, 3, 3, 3, 3, 3, 3, 3, 3, 3, 3, 3, 3, 3, 3, 3, 3, 3, 3, 3, 3, 3, 3, 3, 3, 3, 3, 3, 3, 3, 3, 3, 3, 3, 3, 3, 3, 3, 3, 3, 3, 3, 3, 3, 3, 3, 3, 3, 3, 3, 3, 3, 3, 3, 3, 3, 3, 4 ),
 ( 3.925670666076010412E-10, 0.006134969684172960139, 0.01226993897578289999, 0.01250000110578649952, 0.01840490826738569799, 0.02453987755898860007, 0.02874999196542460042, 0.03067484685060149763, 0.03680981614220439624, 0.04294478543380729485, 0.04500001148800239492, 0.04907975472542019935, 0.05521472401702309796, 0.06124999979532610300, 0.06134969330862600351, 0.06748466260023890106, 0.07361963189184179968, 0.07749999361584829216, 0.07975460118344469829, 0.08588957047505760278, 0.09202453976666050139, 0.09375001134813680526, 0.09815950905826340001, 0.1042944783498659933, 0.1099999977686790115, 0.1104294476415189907, 0.1165644169330719987, 0.1226993862247249961, 0.1262499965223490006, 0.1288343555162780041, 0.1349693248079310015, 0.1411042940994839956, 0.1425000097258770082, 0.1472392633911369930, 0.1533742326826889879, 0.1587499949892519913, 0.1595092019743420131, 0.1656441712658950072, 0.1717791405575480046, 0.1750000001443519915, 0.1779141098491009987, 0.1840490791407540239, 0.1901840484324069935, 0.1912500069742819886, 0.1963190177239599876, 0.2024539870156130128, 0.2074999923037350036, 0.2085889563071649799, 0.2147239255988180051, 0.2208588948903709992, 0.2237500038726649987, 0.2269938641820239966, 0.2331288334735770185, 0.2392638027652299881, 0.2400000037079649817, 0.2453987720567829822, 0.2515337413484359796, 0.2562499904402019690, 0.2576687106399890292, 0.2638036799316419989, 0.2699386492231939938, 0.2725000070773460070, 0.2760736185148470190, 0.2822085878064999886, 0.2883435570980529827, 0.2887500007056810203, 0.2944785263897060079, 0.3006134956812590020, 0.3049999898827670530, 0.3067484649729119717, 0.3128834342644650213, 0.3190184035561179909, 0.3212500092129830231, 0.3251533728476699858, 0.3312883421393230110, 0.3374233114308760051, 0.3435582807225289748, 0.3496932500140820244, 0.3537499908145410044, 0.3558282193057349940, 0.3619631885972879881, 0.3680981578889409578, 0.3700000099152420119, 0.3742331271805939830, 0.3803680964721469770, 0.3862499973465969849, 0.3865030657637990030, 0.3926380350553519971, 0.3987730043470049668, 0.4024999931180490154, 0.4049079736385579609, 0.4110429429302110416, 0.4171779122217639801, 0.4187500090755189586, 0.4233128815134169498, 0.4294478508049699994, 0.4349999948622240153, 0.4355828200966229691, 0.4417177893881750195, 0.4478527586798280447, 0.4512499964198479763, 0.4539877279713809832, 0.4601226972630340084, 0.4662576665546870336, 0.4675000068816390075, 0.4723926358462400277, 0.4785276051378929973, 0.4837499920180829971, 0.4846625744294459914, 0.4907975437210990166, 0.4969325130126520107, 0.5000000001685559470, 0.5030674823043039812, 0.5092024515958569753, 0.5153374208875100004, 0.5162500038123820634, 0.5214723901790629945, 0.5276073594707160197, 0.5324999896260669274, 0.5337423287622690138, 0.5398772980539219279, 0.5460122673455750641, 0.5487500037328389979, 0.5521472366371280582, 0.5582822059287810834, 0.5644171752203329673, 0.5650000005741819820, 0.5705521445119859925, 0.5766871138035389865, 0.5812499883134720768, 0.5828220830951920117, 0.5889570523867450058, 0.5950920216783980310, 0.5975000065084529188, 0.6012269909699510251, 0.6073619602616039392, 0.6134969295531559341, 0.6137499979673349815, 0.6196318988448089593, 0.6257668681363620644, 0.6299999884298229658, 0.6319018374280149786, 0.6380368067196680038, 0.6441717760112209978, 0.6462500080219170107, 0.6503067453028739120, 0.6564417145944269061, 0.6625766838860800423, 0.6687116531776330364, 0.6748466224692860616, 0.6787499900177470513, 0.6809815917608379454, 0.6871165610524909706, 0.6932515303440439647, 0.6950000080182459072, 0.6993864996356971009, 0.7055214689272500950, 0.7112499946371489967, 0.7116564382189030091, 0.7177914075104560032, 0.7239263768021090284, 0.7274999928349140665, 0.7300613460937620536, 0.7361963153853140485, 0.7423312846769670736, 0.7437500065219889711, 0.7484662539685200677, 0.7546012232601729819, 0.7599999918748050476, 0.7607361925517259760, 0.7668711618433790012, 0.7730061311349319952, 0.7762499964153849463, 0.7791411004265850204, 0.7852760697181370153, 0.7914110390097899295, 0.7925000038579510520, 0.7975460083013429236, 0.8036809775929959487, 0.8087499891400269370, 0.8098159468845489428, 0.8159509161762020790, 0.8220858854678549932, 0.8250000001582830089, 0.8282208547594079873, 0.8343558240510610124, 0.8404907933426140065, 0.8412500006211290904, 0.8466257626342659215, 0.8527607319258190266, 0.8574999871756959768, 0.8588957012174720518, 0.8650306705090250459, 0.8711656398006779600, 0.8737500034313691044, 0.8773006090922309541, 0.8834355783838840903, 0.8895705476754370844, 0.8899999975822959764, 0.8957055169670899986, 0.9018404862586419934, 0.9062499864893789336, 0.9079754555502950186, 0.9141104248419479328, 0.9202453941335010379, 0.9225000056768799528, 0.9263803634251540631, 0.9325153327167070572, 0.9386503020083599713, 0.9387499955187870171, 0.9447852712999129654, 0.9509202405915659906, 0.9549999872948490287, 0.9570552098831189847, 0.9631901791747710107, 0.9693251484663240047, 0.9712500064484830276, 0.9754601177579770299, 0.9815950870495300240, 0.9874999942073410253, 0.9877300563411829382, 0.9938650256327359322, 0.9999999949243889574 ),
 .UNSPECIFIED. ) ;
#3225 = CARTESIAN_POINT ( 'NONE',  ( 10.30870223385876372, 21.38393516060608945, -0.7694343885214717238 ) ) ;
#3226 = VERTEX_POINT ( 'NONE', #6905 ) ;
#3227 = CIRCLE ( 'NONE', #14540, 0.3962400000000008138 ) ;
#3228 = CIRCLE ( 'NONE', #20150, 1.983740000000001391 ) ;
#3229 = CARTESIAN_POINT ( 'NONE',  ( 7.744129980428262172, 21.62877852693285874, 3.774467130889562316 ) ) ;
#3230 = LINE ( 'NONE', #3119, #15881 ) ;
#3231 = CARTESIAN_POINT ( 'NONE',  ( 1.169308704210513694, 33.32892749999999893, -20.81168733838920915 ) ) ;
#3232 = VECTOR ( 'NONE', #4382, 1000.000000000000000 ) ;
#3233 = FACE_OUTER_BOUND ( 'NONE', #1743, .T. ) ;
#3234 = VECTOR ( 'NONE', #13395, 1000.000000000000000 ) ;
#3235 = CARTESIAN_POINT ( 'NONE',  ( 6.585898268469219552, 32.54502000000000095, 4.694966092919240275 ) ) ;
#3236 = EDGE_LOOP ( 'NONE', ( #18762, #4860, #20086, #3764 ) ) ;
#3237 = VECTOR ( 'NONE', #912, 1000.000000000000000 ) ;
#3238 = CARTESIAN_POINT ( 'NONE',  ( 9.910007369255215082, 12.06055924076114216, -1.458087275941579275 ) ) ;
#3239 = CLOSED_SHELL ( 'NONE', ( #3186, #21303, #2224, #12793, #3616, #20570 ) ) ;
#3240 = CARTESIAN_POINT ( 'NONE',  ( 2.565001838803366407, 20.83040400030756345, 6.599755016110631090 ) ) ;
#3241 = FACE_OUTER_BOUND ( 'NONE', #21137, .T. ) ;
#3242 = ADVANCED_FACE ( 'NONE', ( #11996 ), #1923, .T. ) ;
#3243 = AXIS2_PLACEMENT_3D ( 'NONE', #3108, #21783, #16394 ) ;
#3244 = CARTESIAN_POINT ( 'NONE',  ( 48.58367710892853353, 0.000000000000000000, -25.32442392637788231 ) ) ;
#3245 = DIRECTION ( 'NONE',  ( -0.8609107660235849613, 0.000000000000000000, 0.5087559856598092844 ) ) ;
#3246 = CARTESIAN_POINT ( 'NONE',  ( 39.55018955470821140, 39.86562041721325045, -3.343445860290124028 ) ) ;
#3247 = CARTESIAN_POINT ( 'NONE',  ( 12.14585711117796230, -6.728073091731484823, -16.90832145949149279 ) ) ;
#3248 = DIRECTION ( 'NONE',  ( 0.000000000000000000, 1.000000000000000000, 0.000000000000000000 ) ) ;
#3249 = CIRCLE ( 'NONE', #17383, 9.524999999999998579 ) ;
#3250 = ORIENTED_EDGE ( 'NONE', *, *, #18507, .F. ) ;
#3251 = CARTESIAN_POINT ( 'NONE',  ( 47.80475250345343596, 42.06303499999999929, -11.91473563638196786 ) ) ;
#3252 = AXIS2_PLACEMENT_3D ( 'NONE', #10278, #10170, #10066 ) ;
#3253 = CARTESIAN_POINT ( 'NONE',  ( 11.01422740109451937, 12.78785806401926095, 5.371526240743504488 ) ) ;
#3254 = DIRECTION ( 'NONE',  ( 0.000000000000000000, 1.000000000000000000, 0.000000000000000000 ) ) ;
#3255 = ORIENTED_EDGE ( 'NONE', *, *, #3436, .T. ) ;
#3256 = CARTESIAN_POINT ( 'NONE',  ( 13.10878000956375722, 16.62975971659733787, 6.403471165590654657 ) ) ;
#3257 = DIRECTION ( 'NONE',  ( 0.000000000000000000, 1.000000000000000000, 0.000000000000000000 ) ) ;
#3258 = DIRECTION ( 'NONE',  ( -0.9579671649362032637, 0.000000000000000000, 0.2868778675745010664 ) ) ;
#3259 = CARTESIAN_POINT ( 'NONE',  ( 17.12141331269406308, -7.465979233334057774, -15.36350049579159638 ) ) ;
#3261 = DIRECTION ( 'NONE',  ( 0.08420877549337300871, 0.000000000000000000, 0.9964481331860212121 ) ) ;
#3260 = CARTESIAN_POINT ( 'NONE',  ( -0.6063867502221114147, 20.39392809349225999, 4.918772829083649434 ) ) ;
#3262 = EDGE_LOOP ( 'NONE', ( #11490, #3775, #11036, #12402 ) ) ;
#3263 = CARTESIAN_POINT ( 'NONE',  ( 0.000000000000000000, 0.000000000000000000, 0.000000000000000000 ) ) ;
#3264 = CARTESIAN_POINT ( 'NONE',  ( -0.1849527129589544072, 21.03045532914853055, 5.150944214860931680 ) ) ;
#3265 = CIRCLE ( 'NONE', #20890, 0.7950200000000005041 ) ;
#3266 = CARTESIAN_POINT ( 'NONE',  ( 3.902814694466206102, 17.50837036387243373, -0.5262828315819897407 ) ) ;
#3267 = AXIS2_PLACEMENT_3D ( 'NONE', #16888, #1957, #11705 ) ;
#3268 = VERTEX_POINT ( 'NONE', #3706 ) ;
#3269 = DIRECTION ( 'NONE',  ( 0.2490110332224850231, 0.000000000000000000, -0.9685006480810791629 ) ) ;
#3270 = AXIS2_PLACEMENT_3D ( 'NONE', #6464, #9767, #6780 ) ;
#3271 = CARTESIAN_POINT ( 'NONE',  ( 17.57968847865632611, -8.559078652989546399, -15.87053422043189421 ) ) ;
#3272 = ORIENTED_EDGE ( 'NONE', *, *, #18097, .T. ) ;
#3273 = MECHANICAL_DESIGN_GEOMETRIC_PRESENTATION_REPRESENTATION (  '', ( #11042 ), #7510 ) ;
#3274 = CARTESIAN_POINT ( 'NONE',  ( 9.246163857139698905, 15.41858152414332750, -2.865988929752159464 ) ) ;
#3275 = CARTESIAN_POINT ( 'NONE',  ( 1.998220421679061776, 5.548947500000001476, -22.64748046904500356 ) ) ;
#3276 = CARTESIAN_POINT ( 'NONE',  ( 8.395333527031370480, 21.35108299968154455, -0.1513204485400149457 ) ) ;
#3277 = ADVANCED_FACE ( 'NONE', ( #13777 ), #3596, .T. ) ;
#3278 = AXIS2_PLACEMENT_3D ( 'NONE', #626, #19199, #17553 ) ;
#3279 = CARTESIAN_POINT ( 'NONE',  ( 17.54816828402311302, -6.930789574793553065, -15.75670520605582858 ) ) ;
#3280 =( NAMED_UNIT ( * ) SI_UNIT ( $, .STERADIAN. ) SOLID_ANGLE_UNIT ( ) );
#3281 = EDGE_LOOP ( 'NONE', ( #15040, #14651, #4050, #19861 ) ) ;
#3282 = CARTESIAN_POINT ( 'NONE',  ( 10.10356450120315763, 20.54903548560601578, 4.403050154276548334 ) ) ;
#3283 = CARTESIAN_POINT ( 'NONE',  ( 12.00018126865166401, 10.33025398667194139, 0.6449774946455864022 ) ) ;
#3284 = LINE ( 'NONE', #1502, #22 ) ;
#3285 = ORIENTED_EDGE ( 'NONE', *, *, #1514, .T. ) ;
#3286 = ORIENTED_EDGE ( 'NONE', *, *, #9816, .F. ) ;
#3287 = VECTOR ( 'NONE', #7685, 1000.000000000000114 ) ;
#3288 = DIRECTION ( 'NONE',  ( -0.9685006480810791629, 0.000000000000000000, -0.2490110332224850509 ) ) ;
#3289 = AXIS2_PLACEMENT_3D ( 'NONE', #1672, #10086, #3454 ) ;
#3291 = FACE_OUTER_BOUND ( 'NONE', #2741, .T. ) ;
#3290 = CARTESIAN_POINT ( 'NONE',  ( 3.171475446957850775, 11.89587513260652152, 6.915618804319352719 ) ) ;
#3292 = ORIENTED_EDGE ( 'NONE', *, *, #8367, .T. ) ;
#3293 = CARTESIAN_POINT ( 'NONE',  ( 6.634334687536620478, 20.47748668554710960, 6.460578472925798899 ) ) ;
#3294 = VERTEX_POINT ( 'NONE', #15441 ) ;
#3295 = EDGE_LOOP ( 'NONE', ( #17508, #19503, #2757, #7196 ) ) ;
#3296 = EDGE_CURVE ( 'NONE', #10564, #3737, #11811, .T. ) ;
#3297 = CIRCLE ( 'NONE', #19863, 3.970019999999998550 ) ;
#3298 = DIRECTION ( 'NONE',  ( 0.7421532822901580895, -0.000000000000000000, -0.6702301885068630005 ) ) ;
#3299 = ORIENTED_EDGE ( 'NONE', *, *, #989, .T. ) ;
#3300 = CARTESIAN_POINT ( 'NONE',  ( 11.86776211864144770, 20.19146305430580313, -3.151330312819546453 ) ) ;
#3301 = EDGE_CURVE ( 'NONE', #5598, #1715, #13903, .T. ) ;
#3302 = AXIS2_PLACEMENT_3D ( 'NONE', #7216, #8851, #7091 ) ;
#3303 =( GEOMETRIC_REPRESENTATION_CONTEXT ( 3 ) GLOBAL_UNCERTAINTY_ASSIGNED_CONTEXT ( ( #10781 ) ) GLOBAL_UNIT_ASSIGNED_CONTEXT ( ( #3721, #20834, #13917 ) ) REPRESENTATION_CONTEXT ( 'NONE', 'WORKASPACE' ) );
#3304 = EDGE_CURVE ( 'NONE', #13139, #4078, #5458, .T. ) ;
#3305 = FACE_OUTER_BOUND ( 'NONE', #9165, .T. ) ;
#3306 = CARTESIAN_POINT ( 'NONE',  ( 17.34610635302146164, 19.43957250000000059, -18.70138818597152053 ) ) ;
#3307 = CARTESIAN_POINT ( 'NONE',  ( 2.006824028408880967, 12.19579955713188646, 1.406014205417876806 ) ) ;
#3308 = ORIENTED_EDGE ( 'NONE', *, *, #16549, .T. ) ;
#3309 = DIRECTION ( 'NONE',  ( 0.9999603561554373243, 0.000000000000000000, -0.008904275236710241376 ) ) ;
#3310 = CARTESIAN_POINT ( 'NONE',  ( 11.97174136233939556, 21.25996874134203551, -17.62449286037261942 ) ) ;
#3311 = CARTESIAN_POINT ( 'NONE',  ( 28.97711086133420366, 30.56064500000000095, -10.31874999999999964 ) ) ;
#3312 = CARTESIAN_POINT ( 'NONE',  ( -15.39353573898878658, -4.587157632697119958, -10.30107656633069979 ) ) ;
#3313 = AXIS2_PLACEMENT_3D ( 'NONE', #14147, #10473, #7374 ) ;
#3314 = ORIENTED_EDGE ( 'NONE', *, *, #3919, .T. ) ;
#3315 = ORIENTED_EDGE ( 'NONE', *, *, #9816, .T. ) ;
#3316 = CARTESIAN_POINT ( 'NONE',  ( 11.40924028808832524, 19.77353779035612291, -2.514324500111221994 ) ) ;
#3317 = CARTESIAN_POINT ( 'NONE',  ( 22.22454659879084460, 36.51313500000000545, -13.75904720189594244 ) ) ;
#3318 = VERTEX_POINT ( 'NONE', #11101 ) ;
#3319 = ORIENTED_EDGE ( 'NONE', *, *, #18555, .T. ) ;
#3320 = CARTESIAN_POINT ( 'NONE',  ( 1.268730000000000135, 23.41816500000000190, 10.65596716962832069 ) ) ;
#3321 = AXIS2_PLACEMENT_3D ( 'NONE', #15568, #20180, #13579 ) ;
#3322 = ORIENTED_EDGE ( 'NONE', *, *, #12917, .T. ) ;
#3323 = ADVANCED_FACE ( 'NONE', ( #14009 ), #5801, .T. ) ;
#3324 = CARTESIAN_POINT ( 'NONE',  ( 9.272449929266908697, 15.41853785818361366, 7.143357861250589913 ) ) ;
#3325 = AXIS2_PLACEMENT_3D ( 'NONE', #21773, #6624, #15160 ) ;
#3326 = DIRECTION ( 'NONE',  ( 0.000000000000000000, 1.000000000000000000, 0.000000000000000000 ) ) ;
#3327 = CYLINDRICAL_SURFACE ( 'NONE', #3325, 0.5953125000000004663 ) ;
#3328 = FACE_OUTER_BOUND ( 'NONE', #7245, .T. ) ;
#3329 = DIRECTION ( 'NONE',  ( 0.000000000000000000, -1.000000000000000000, -0.000000000000000000 ) ) ;
#3330 = CARTESIAN_POINT ( 'NONE',  ( 0.2584401386766148612, 11.97670218361793282, 2.636262851981420408 ) ) ;
#3331 = ORIENTED_EDGE ( 'NONE', *, *, #14696, .T. ) ;
#3332 = CARTESIAN_POINT ( 'NONE',  ( 3.848227522671471501, 14.05442396375854130, -0.1621833816910843162 ) ) ;
#3333 = VECTOR ( 'NONE', #4968, 1000.000000000000227 ) ;
#3334 = DIRECTION ( 'NONE',  ( 0.000000000000000000, 0.000000000000000000, -1.000000000000000000 ) ) ;
#3335 = CARTESIAN_POINT ( 'NONE',  ( 52.69088350064333781, -7.396940496609654581, -17.13629674769522282 ) ) ;
#3336 = SURFACE_SIDE_STYLE ('',( #12058 ) ) ;
#3337 = DIRECTION ( 'NONE',  ( -0.2145948757085689163, -0.000000000000000000, -0.9767031480033347979 ) ) ;
#3338 = VERTEX_POINT ( 'NONE', #17746 ) ;
#3339 = CARTESIAN_POINT ( 'NONE',  ( 11.09713900613744286, 13.72201164258680173, 7.095940182945178698 ) ) ;
#3340 = CARTESIAN_POINT ( 'NONE',  ( -7.949728765565600597, -0.7997824999999986195, -34.47798802950714503 ) ) ;
#3341 = CARTESIAN_POINT ( 'NONE',  ( 13.23764915724263247, 17.68517305658646421, 7.025134865669341977 ) ) ;
#3342 = ORIENTED_EDGE ( 'NONE', *, *, #18833, .F. ) ;
#3343 = CIRCLE ( 'NONE', #19912, 5.357812499999999645 ) ;
#3344 = CARTESIAN_POINT ( 'NONE',  ( 7.493139529700894030, 21.70524941769282989, 3.085289908977460804 ) ) ;
#3345 = DIRECTION ( 'NONE',  ( 0.6744690509234934073, 0.7360996206939023345, -0.05699866455150641442 ) ) ;
#3346 = FACE_OUTER_BOUND ( 'NONE', #7256, .T. ) ;
#3347 = ADVANCED_FACE ( 'NONE', ( #7673 ), #12323, .T. ) ;
#3348 =( NAMED_UNIT ( * ) SI_UNIT ( $, .STERADIAN. ) SOLID_ANGLE_UNIT ( ) );
#3349 = CARTESIAN_POINT ( 'NONE',  ( 7.058968441123867343, 18.03812148340534094, 7.310900384194754409 ) ) ;
#3350 = EDGE_CURVE ( 'NONE', #21216, #18977, #15715, .T. ) ;
#3351 = PLANE ( 'NONE',  #18829 ) ;
#3352 = CIRCLE ( 'NONE', #4412, 0.7950200000000000600 ) ;
#3353 = LINE ( 'NONE', #15082, #4579 ) ;
#3354 = CARTESIAN_POINT ( 'NONE',  ( 7.168925875378048040, 11.43880029099476126, 4.249497758341346021 ) ) ;
#3355 = AXIS2_PLACEMENT_3D ( 'NONE', #14168, #12500, #15603 ) ;
#3356 = DIRECTION ( 'NONE',  ( 0.000000000000000000, 1.000000000000000000, 0.000000000000000000 ) ) ;
#3357 = CARTESIAN_POINT ( 'NONE',  ( 3.384013584124889729, 18.28285541323128172, 8.939367623630410264 ) ) ;
#3358 = CARTESIAN_POINT ( 'NONE',  ( -53.00154558624916490, 38.26001999999999725, -22.85927301266823264 ) ) ;
#3359 = CARTESIAN_POINT ( 'NONE',  ( 11.56192577415882816, -3.968114999999999615, 4.677561850332325299 ) ) ;
#3360 = CARTESIAN_POINT ( 'NONE',  ( -1.351150467732365579, 28.56769750000000130, -27.17319717629097653 ) ) ;
#3361 = DIRECTION ( 'NONE',  ( 0.000000000000000000, 1.000000000000000000, 0.000000000000000000 ) ) ;
#3362 = CARTESIAN_POINT ( 'NONE',  ( 39.44573040579900436, 39.95099742452212865, -3.441431441669689395 ) ) ;
#3363 = CARTESIAN_POINT ( 'NONE',  ( 11.30579500508379809, -5.488445583102078196, -17.06917961439425824 ) ) ;
#3364 = VERTEX_POINT ( 'NONE', #20817 ) ;
#3365 = CARTESIAN_POINT ( 'NONE',  ( 11.37517772858290677, 16.82229854605489550, 7.558283270811076981 ) ) ;
#3366 = ORIENTED_EDGE ( 'NONE', *, *, #13040, .F. ) ;
#3367 = CARTESIAN_POINT ( 'NONE',  ( 13.14561042020424075, 14.29266759713506652, 6.004341513937229813 ) ) ;
#3368 = CARTESIAN_POINT ( 'NONE',  ( 12.46105965416778716, -5.663837116554884865, -16.83730257442121214 ) ) ;
#3370 = DIRECTION ( 'NONE',  ( -0.1060008583745224581, 0.000000000000000000, -0.9943660382494288186 ) ) ;
#3369 = CARTESIAN_POINT ( 'NONE',  ( 4.635123512035450588, 12.02159401923784010, 5.456644224042059399 ) ) ;
#3371 = VERTEX_POINT ( 'NONE', #17855 ) ;
#3372 = VECTOR ( 'NONE', #13803, 1000.000000000000114 ) ;
#3373 = CARTESIAN_POINT ( 'NONE',  ( 46.03750000000000142, -9.531985000000000596, -10.31874999999999964 ) ) ;
#3374 = ADVANCED_FACE ( 'NONE', ( #17629 ), #6006, .T. ) ;
#3375 = LINE ( 'NONE', #17178, #645 ) ;
#3376 = DIRECTION ( 'NONE',  ( 0.000000000000000000, -1.000000000000000000, -0.000000000000000000 ) ) ;
#3377 = ORIENTED_EDGE ( 'NONE', *, *, #851, .F. ) ;
#3378 = CARTESIAN_POINT ( 'NONE',  ( 13.49155064010361471, 21.41280428856536489, 2.268588950130180582 ) ) ;
#3379 = CARTESIAN_POINT ( 'NONE',  ( 11.22736586087230393, 14.04501930844190660, 6.381908989529498477 ) ) ;
#3380 = CARTESIAN_POINT ( 'NONE',  ( 38.57962667713734817, 37.84782743281653694, -4.391981920076847068 ) ) ;
#3381 = CARTESIAN_POINT ( 'NONE',  ( 9.493963008126993230, 14.64601895156848776, 7.857208408461620053 ) ) ;
#3382 = VECTOR ( 'NONE', #16625, 1000.000000000000227 ) ;
#3383 = CARTESIAN_POINT ( 'NONE',  ( 11.89504694164775422, -2.569623862214921228, -16.80242428561735935 ) ) ;
#3384 = CARTESIAN_POINT ( 'NONE',  ( 2.063750000000000195, 2.380615000000000148, 8.731249999999999289 ) ) ;
#3385 = ORIENTED_EDGE ( 'NONE', *, *, #14955, .T. ) ;
#3386 = CARTESIAN_POINT ( 'NONE',  ( 10.37956912121652131, 20.06616296009919864, 5.118516414627194422 ) ) ;
#3387 = CARTESIAN_POINT ( 'NONE',  ( 11.19977597401542901, 12.02381550237932295, 5.862906665875985190 ) ) ;
#3388 = DIRECTION ( 'NONE',  ( -0.9987059298363657467, 0.000000000000000000, -0.05085730733808445370 ) ) ;
#3389 = ORIENTED_EDGE ( 'NONE', *, *, #16792, .T. ) ;
#3390 = ORIENTED_EDGE ( 'NONE', *, *, #5399, .F. ) ;
#3391 = CARTESIAN_POINT ( 'NONE',  ( 53.12464125271250737, -5.166565464015373976, -16.68257730012009077 ) ) ;
#3392 = CARTESIAN_POINT ( 'NONE',  ( 10.93899656833006695, 16.07662961819365677, -4.343109068444145571 ) ) ;
#3394 = DIRECTION ( 'NONE',  ( 1.000000000000000000, 0.000000000000000000, 0.000000000000000000 ) ) ;
#3393 = CARTESIAN_POINT ( 'NONE',  ( 1.795302335458940579, 11.90891113418242142, 1.891703290912318147 ) ) ;
#3395 = ORIENTED_EDGE ( 'NONE', *, *, #11430, .F. ) ;
#3396 = CARTESIAN_POINT ( 'NONE',  ( 6.271597670968151128, 21.07808100295144982, 5.497337236915185166 ) ) ;
#3397 = EDGE_CURVE ( 'NONE', #5196, #8930, #13238, .T. ) ;
#3398 = ORIENTED_EDGE ( 'NONE', *, *, #16484, .F. ) ;
#3399 = CARTESIAN_POINT ( 'NONE',  ( 24.26606285357373594, 29.75832250000000201, -16.92219937337620195 ) ) ;
#3400 = ORIENTED_EDGE ( 'NONE', *, *, #21525, .F. ) ;
#3401 = CARTESIAN_POINT ( 'NONE',  ( 1.917016422406038645, 14.23731939350392217, 0.6161444402295471745 ) ) ;
#3402 = DIRECTION ( 'NONE',  ( -1.000000000000000000, 0.000000000000000000, 0.000000000000000000 ) ) ;
#3403 = DIRECTION ( 'NONE',  ( 0.000000000000000000, -1.000000000000000000, 0.000000000000000000 ) ) ;
#3404 = CARTESIAN_POINT ( 'NONE',  ( 22.22454659879084460, 36.51313500000000545, -13.75904720189594244 ) ) ;
#3405 = CARTESIAN_POINT ( 'NONE',  ( 2.061500982823199823, 18.90949574706995406, -0.05049993479792989209 ) ) ;
#3406 = VERTEX_POINT ( 'NONE', #14433 ) ;
#3407 = DIRECTION ( 'NONE',  ( -1.000000000000000000, 0.000000000000000000, 0.000000000000000000 ) ) ;
#3408 = CARTESIAN_POINT ( 'NONE',  ( 65.67421548912699336, 0.000000000000000000, -10.93409647675949969 ) ) ;
#3409 = DIRECTION ( 'NONE',  ( -0.2490110332224848289, 0.000000000000000000, 0.9685006480810792739 ) ) ;
#3410 = EDGE_CURVE ( 'NONE', #2524, #14810, #14658, .T. ) ;
#3411 = CARTESIAN_POINT ( 'NONE',  ( 46.03750000000000142, 32.54502000000000095, -10.31874999999999964 ) ) ;
#3413 = CARTESIAN_POINT ( 'NONE',  ( 19.59062520529572993, -4.350225641996413373, -14.17140907119074988 ) ) ;
#3412 = CARTESIAN_POINT ( 'NONE',  ( 52.44708915697334106, 32.54502000000000095, 4.020247972991190188 ) ) ;
#3414 = VERTEX_POINT ( 'NONE', #10990 ) ;
#3415 = ORIENTED_EDGE ( 'NONE', *, *, #17099, .T. ) ;
#3416 = CARTESIAN_POINT ( 'NONE',  ( 11.21942781118996990, 21.35256525590422072, 2.014744391537809598 ) ) ;
#3417 = ORIENTED_EDGE ( 'NONE', *, *, #14010, .F. ) ;
#3418 = ORIENTED_EDGE ( 'NONE', *, *, #6294, .T. ) ;
#3419 = FACE_OUTER_BOUND ( 'NONE', #2151, .T. ) ;
#3420 = EDGE_CURVE ( 'NONE', #12389, #6378, #8643, .T. ) ;
#3421 = ORIENTED_EDGE ( 'NONE', *, *, #3725, .F. ) ;
#3422 = EDGE_CURVE ( 'NONE', #14476, #21616, #11099, .T. ) ;
#3423 = CARTESIAN_POINT ( 'NONE',  ( 8.349616978403640033, 11.53155059953441075, 2.515314769403827366 ) ) ;
#3424 = CARTESIAN_POINT ( 'NONE',  ( 3.429437941603723505, 15.04225738252103461, 8.249934406976112911 ) ) ;
#3425 = CARTESIAN_POINT ( 'NONE',  ( 59.89111109153450485, -1.983739999999999837, -22.14529389979288965 ) ) ;
#3426 = PLANE ( 'NONE',  #15712 ) ;
#3427 = DIRECTION ( 'NONE',  ( 0.8609107660235850723, 0.000000000000000000, -0.5087559856598092844 ) ) ;
#3428 = CARTESIAN_POINT ( 'NONE',  ( -0.02301601734996851917, 17.64104708308499880, 0.1929137087451379406 ) ) ;
#3429 = CYLINDRICAL_SURFACE ( 'NONE', #20028, 0.7950200000000003930 ) ;
#3430 = AXIS2_PLACEMENT_3D ( 'NONE', #10247, #15695, #13929 ) ;
#3431 = VERTEX_POINT ( 'NONE', #9328 ) ;
#3432 = CARTESIAN_POINT ( 'NONE',  ( 3.509439300273259565, 17.99578554531247576, 8.209304056720553078 ) ) ;
#3433 = CARTESIAN_POINT ( 'NONE',  ( 13.48619406898445661, -14.84248999999999974, -16.00576350138265624 ) ) ;
#3434 = LINE ( 'NONE', #13727, #2530 ) ;
#3435 =( LENGTH_UNIT ( ) NAMED_UNIT ( * ) SI_UNIT ( .MILLI., .METRE. ) );
#3436 = EDGE_CURVE ( 'NONE', #1617, #13806, #10759, .T. ) ;
#3437 = DIRECTION ( 'NONE',  ( -0.9964481331860213231, 0.000000000000000000, 0.08420877549337306422 ) ) ;
#3438 = ORIENTED_EDGE ( 'NONE', *, *, #18458, .F. ) ;
#3439 = CARTESIAN_POINT ( 'NONE',  ( 7.252818009422052903, 21.72673311005876329, 3.332971805317985758 ) ) ;
#3440 = CARTESIAN_POINT ( 'NONE',  ( -49.72082486877479113, -5.714364999999999029, -7.603226040068017610 ) ) ;
#3441 = CARTESIAN_POINT ( 'NONE',  ( 13.02404159230300174, 18.96437007834888888, 6.572007044681392074 ) ) ;
#3442 = ORIENTED_EDGE ( 'NONE', *, *, #16622, .F. ) ;
#3443 = CARTESIAN_POINT ( 'NONE',  ( 9.484727789049149038, 14.55342286457404555, 7.702955061670587966 ) ) ;
#3444 = CARTESIAN_POINT ( 'NONE',  ( 6.206528234269004685, 20.44464562225766358, 5.215226569823482983 ) ) ;
#3445 = CYLINDRICAL_SURFACE ( 'NONE', #2769, 3.970020000000001215 ) ;
#3446 = EDGE_CURVE ( 'NONE', #5914, #20066, #19279, .T. ) ;
#3447 = CARTESIAN_POINT ( 'NONE',  ( 31.02798609601340729, 34.52875999999999834, -5.485920235548950252 ) ) ;
#3448 = VECTOR ( 'NONE', #955, 1000.000000000000000 ) ;
#3449 = FACE_OUTER_BOUND ( 'NONE', #8597, .T. ) ;
#3450 = DIRECTION ( 'NONE',  ( 0.05085730733808393328, 0.000000000000000000, -0.9987059298363656357 ) ) ;
#3451 = CARTESIAN_POINT ( 'NONE',  ( 7.965518406716108224, 21.40982604368873865, 3.095704102008969283 ) ) ;
#3452 = CARTESIAN_POINT ( 'NONE',  ( 5.376417996899292895, 15.42671590247574542, 7.949579020774653060 ) ) ;
#3453 = CARTESIAN_POINT ( 'NONE',  ( 5.957292673923675785, 11.58109048093756321, 0.5680188385854727517 ) ) ;
#3454 = DIRECTION ( 'NONE',  ( 0.9997303917939455165, 0.000000000000000000, 0.02321946863139149123 ) ) ;
#3455 = CARTESIAN_POINT ( 'NONE',  ( 20.21692672805859559, -1.125648057385024270, -14.76250352900288298 ) ) ;
#3456 = CARTESIAN_POINT ( 'NONE',  ( 2.812310173516594958, 12.03281576442448042, 5.089945059218950796 ) ) ;
#3457 = DIRECTION ( 'NONE',  ( 0.6702301885068652210, 0.000000000000000000, 0.7421532822901560911 ) ) ;
#3458 = CARTESIAN_POINT ( 'NONE',  ( 18.38276939006084731, -7.844924378857746738, -15.55834805662867737 ) ) ;
#3459 = EDGE_CURVE ( 'NONE', #4834, #6054, #5436, .T. ) ;
#3460 = EDGE_CURVE ( 'NONE', #10436, #20642, #13949, .T. ) ;
#3461 =( LENGTH_UNIT ( ) NAMED_UNIT ( * ) SI_UNIT ( .MILLI., .METRE. ) );
#3462 = EDGE_CURVE ( 'NONE', #7874, #4463, #8363, .T. ) ;
#3463 = TOROIDAL_SURFACE ( 'NONE', #633, 3.174999999999999822, 1.190625000000000044 ) ;
#3464 = VERTEX_POINT ( 'NONE', #11638 ) ;
#3465 = CARTESIAN_POINT ( 'NONE',  ( 9.621872815474498353, 21.81549092655993860, 3.148079541620338428 ) ) ;
#3466 = DIRECTION ( 'NONE',  ( 0.05085730733808393328, 0.000000000000000000, -0.9987059298363656357 ) ) ;
#3467 = ORIENTED_EDGE ( 'NONE', *, *, #18533, .T. ) ;
#3468 = CARTESIAN_POINT ( 'NONE',  ( 12.91587739171063021, 18.12504211422740141, 6.097017937141830934 ) ) ;
#3469 = CARTESIAN_POINT ( 'NONE',  ( 19.40594143866619703, -5.840264277364781265, -15.43021847716318717 ) ) ;
#3471 = DIRECTION ( 'NONE',  ( 0.9959941601142464629, 0.000000000000000000, 0.08941830359784717908 ) ) ;
#3470 = CARTESIAN_POINT ( 'NONE',  ( 3.788989557899201888, 18.74075759514924400, -0.1305876994136269953 ) ) ;
#3472 = ORIENTED_EDGE ( 'NONE', *, *, #8565, .T. ) ;
#3473 = CARTESIAN_POINT ( 'NONE',  ( -22.90765545213488963, -10.87373999999999974, -9.869178565316103047 ) ) ;
#3474 = DIRECTION ( 'NONE',  ( 0.000000000000000000, 1.000000000000000000, 0.000000000000000000 ) ) ;
#3475 = CARTESIAN_POINT ( 'NONE',  ( 6.308080149185702368, 10.92909866215502213, 2.816645635463620678 ) ) ;
#3476 = AXIS2_PLACEMENT_3D ( 'NONE', #14244, #16222, #14564 ) ;
#3477 = EDGE_LOOP ( 'NONE', ( #9306, #3319, #14708, #12162 ) ) ;
#3478 = CARTESIAN_POINT ( 'NONE',  ( 11.59058392313026076, 11.69902548067542192, -0.9553338480370143770 ) ) ;
#3479 = CARTESIAN_POINT ( 'NONE',  ( 11.16177022631493720, 16.27078869972547892, -3.700522497431344426 ) ) ;
#3480 = CARTESIAN_POINT ( 'NONE',  ( 3.871967422488196142, 13.36420590592894264, 7.787245618273578529 ) ) ;
#3481 = CARTESIAN_POINT ( 'NONE',  ( 11.99291685403952101, 21.69057506433588145, 3.971327024042194509 ) ) ;
#3482 = AXIS2_PLACEMENT_3D ( 'NONE', #14888, #6469, #4816 ) ;
#3483 = CARTESIAN_POINT ( 'NONE',  ( 11.99578385045931839, -4.049420365113250320, -16.84642447179846414 ) ) ;
#3484 = EDGE_CURVE ( 'NONE', #1216, #16869, #14872, .T. ) ;
#3485 = CARTESIAN_POINT ( 'NONE',  ( 10.70549249095554423, -4.788864733378723315, -15.64570743106055062 ) ) ;
#3486 = EDGE_LOOP ( 'NONE', ( #10195, #2685, #263, #12752 ) ) ;
#3487 = CARTESIAN_POINT ( 'NONE',  ( 10.30207946694087262, 20.21713832266318533, 4.919229887006573598 ) ) ;
#3488 = CARTESIAN_POINT ( 'NONE',  ( 13.59613746992887506, 22.20171528482708112, 2.423511226437077948 ) ) ;
#3489 = ORIENTED_EDGE ( 'NONE', *, *, #21038, .F. ) ;
#3490 = EDGE_LOOP ( 'NONE', ( #19039, #9864, #62, #20847 ) ) ;
#3491 = AXIS2_PLACEMENT_3D ( 'NONE', #16476, #8053, #11819 ) ;
#3492 = FACE_OUTER_BOUND ( 'NONE', #771, .T. ) ;
#3493 = CARTESIAN_POINT ( 'NONE',  ( 11.39852134277141360, 19.53005087718068111, -3.485485373183195623 ) ) ;
#3495 = DIRECTION ( 'NONE',  ( -0.3928209820863007296, 0.000000000000000000, 0.9196149607486571176 ) ) ;
#3494 = CARTESIAN_POINT ( 'NONE',  ( 3.137202520011495466, 21.36287299093768155, 3.610942509148120205 ) ) ;
#3496 = ORIENTED_EDGE ( 'NONE', *, *, #114, .T. ) ;
#3497 = CARTESIAN_POINT ( 'NONE',  ( 6.099937697436127237, 21.27555018051177171, 5.034626513405442871 ) ) ;
#3498 = FACE_OUTER_BOUND ( 'NONE', #3983, .T. ) ;
#3499 = ORIENTED_EDGE ( 'NONE', *, *, #1244, .T. ) ;
#3500 = AXIS2_PLACEMENT_3D ( 'NONE', #7043, #8921, #15699 ) ;
#3501 = DIRECTION ( 'NONE',  ( -0.2490110332224850231, 0.000000000000000000, 0.9685006480810791629 ) ) ;
#3502 = ORIENTED_EDGE ( 'NONE', *, *, #3975, .F. ) ;
#3503 = AXIS2_PLACEMENT_3D ( 'NONE', #8893, #608, #21052 ) ;
#3504 = CARTESIAN_POINT ( 'NONE',  ( 61.65536943582333151, 0.000000000000000000, -11.98363747855214712 ) ) ;
#3505 = CYLINDRICAL_SURFACE ( 'NONE', #10583, 30.16249999999999432 ) ;
#3506 = CARTESIAN_POINT ( 'NONE',  ( -15.84345693979480352, 37.60427460010093625, -10.46616649349356365 ) ) ;
#3507 = CARTESIAN_POINT ( 'NONE',  ( 1.684397325192768413, 16.20931629175901634, -0.6950957481128374749 ) ) ;
#3508 = EDGE_CURVE ( 'NONE', #15795, #20381, #21264, .T. ) ;
#3509 = CARTESIAN_POINT ( 'NONE',  ( 48.78323016782857735, 37.11476346399999926, -25.79158832643865651 ) ) ;
#3510 = AXIS2_PLACEMENT_3D ( 'NONE', #19713, #12669, #11000 ) ;
#3511 = ORIENTED_EDGE ( 'NONE', *, *, #20455, .T. ) ;
#3512 = CARTESIAN_POINT ( 'NONE',  ( 19.99312429566830218, -95.96551800000000298, -11.46559883803463720 ) ) ;
#3513 = CARTESIAN_POINT ( 'NONE',  ( 65.51436440461340283, 32.54502000000000095, -12.87863775929475985 ) ) ;
#3514 = DIRECTION ( 'NONE',  ( 0.000000000000000000, -1.000000000000000000, 0.000000000000000000 ) ) ;
#3515 = CARTESIAN_POINT ( 'NONE',  ( 10.40254502969509964, -3.119958055837774413, -17.26346415963410053 ) ) ;
#3517 = CARTESIAN_POINT ( 'NONE',  ( 12.92878071497339931, -6.147102104778971565, -15.49261626134594572 ) ) ;
#3516 = CARTESIAN_POINT ( 'NONE',  ( 12.11879977990919421, 19.43893749999999798, 0.1373704394269426865 ) ) ;
#3518 = VERTEX_POINT ( 'NONE', #16738 ) ;
#3519 = VERTEX_POINT ( 'NONE', #1149 ) ;
#3520 = CARTESIAN_POINT ( 'NONE',  ( 6.628279328482711286, 11.82958596167992127, 4.306176057588643857 ) ) ;
#3522 = DIRECTION ( 'NONE',  ( -0.6702301885068652210, 0.000000000000000000, -0.7421532822901560911 ) ) ;
#3521 = CARTESIAN_POINT ( 'NONE',  ( 7.459674749802357674, 12.98268228153804138, 7.394826790990479459 ) ) ;
#3523 = ORIENTED_EDGE ( 'NONE', *, *, #7734, .F. ) ;
#3524 = VERTEX_POINT ( 'NONE', #12887 ) ;
#3525 = CARTESIAN_POINT ( 'NONE',  ( 49.15122309515935228, 0.000000000000000000, -25.07506492104907991 ) ) ;
#3526 = SHAPE_REPRESENTATION ( 'Split Webbing Winding Axle', ( #2234 ), #5057 ) ;
#3527 = EDGE_LOOP ( 'NONE', ( #2092, #21268, #2367, #10870 ) ) ;
#3528 = CARTESIAN_POINT ( 'NONE',  ( 7.542404986124462418, 13.51227111306877582, -1.211156836538626713 ) ) ;
#3529 = AXIS2_PLACEMENT_3D ( 'NONE', #12859, #4446, #5157 ) ;
#3530 = FACE_OUTER_BOUND ( 'NONE', #12817, .T. ) ;
#3531 = DIRECTION ( 'NONE',  ( 0.000000000000000000, -1.000000000000000000, -0.000000000000000000 ) ) ;
#3532 = CYLINDRICAL_SURFACE ( 'NONE', #5092, 3.970019999999998550 ) ;
#3533 = DIRECTION ( 'NONE',  ( 0.000000000000000000, 1.000000000000000000, 0.000000000000000000 ) ) ;
#3534 = CARTESIAN_POINT ( 'NONE',  ( -0.005519112348255535150, 12.92290799471926555, 1.396275220874262368 ) ) ;
#3535 = EDGE_CURVE ( 'NONE', #18152, #4527, #4800, .T. ) ;
#3536 = CARTESIAN_POINT ( 'NONE',  ( 32.52436584422698473, 0.000000000000000000, 1.884807767196291284 ) ) ;
#3537 = EDGE_CURVE ( 'NONE', #1050, #7386, #1467, .T. ) ;
#3538 = ORIENTED_EDGE ( 'NONE', *, *, #18968, .T. ) ;
#3539 = CARTESIAN_POINT ( 'NONE',  ( 3.451617604026494757, 12.51757774536594070, 6.438078665016687019 ) ) ;
#3540 = DIRECTION ( 'NONE',  ( 0.000000000000000000, -1.000000000000000000, -0.000000000000000000 ) ) ;
#3541 = CARTESIAN_POINT ( 'NONE',  ( 50.29383871662588490, 32.54502000000000095, -28.02957329025317179 ) ) ;
#3542 = ORIENTED_EDGE ( 'NONE', *, *, #14324, .F. ) ;
#3543 = CARTESIAN_POINT ( 'NONE',  ( 5.749044579667681454, 11.19290776549860134, 1.467727128716227680 ) ) ;
#3544 = VECTOR ( 'NONE', #17324, 1000.000000000000114 ) ;
#3545 = LINE ( 'NONE', #10282, #13496 ) ;
#3546 = CARTESIAN_POINT ( 'NONE',  ( 11.77504171138678579, 21.82382164323249185, 3.283033003548121886 ) ) ;
#3547 = VERTEX_POINT ( 'NONE', #13104 ) ;
#3548 = VECTOR ( 'NONE', #20949, 1000.000000000000000 ) ;
#3549 = ORIENTED_EDGE ( 'NONE', *, *, #8954, .F. ) ;
#3550 = DIRECTION ( 'NONE',  ( 0.000000000000000000, 1.000000000000000000, 0.000000000000000000 ) ) ;
#3551 = CARTESIAN_POINT ( 'NONE',  ( 9.488210770742556477, 14.67898782071606689, 7.740838414784177779 ) ) ;
#3552 = CARTESIAN_POINT ( 'NONE',  ( 6.695256992210804725, 11.71104153968872197, 4.085482631342693516 ) ) ;
#3553 = CARTESIAN_POINT ( 'NONE',  ( -29.36874999999999858, 1.983739999999999837, 10.71562499999999929 ) ) ;
#3554 = CARTESIAN_POINT ( 'NONE',  ( 1.952969610814715207, 74.97070807199999365, 6.747510000000000119 ) ) ;
#3555 = VECTOR ( 'NONE', #14730, 1000.000000000000000 ) ;
#3556 = CARTESIAN_POINT ( 'NONE',  ( 1.355844778331848799, 20.27946762757392563, 3.649167961216476463 ) ) ;
#3557 = CIRCLE ( 'NONE', #7453, 0.5079999999999996740 ) ;
#3558 = CARTESIAN_POINT ( 'NONE',  ( -15.60052840353448644, 34.87627845846405705, -10.41609846181108345 ) ) ;
#3559 = EDGE_CURVE ( 'NONE', #1126, #15606, #5100, .T. ) ;
#3560 = CARTESIAN_POINT ( 'NONE',  ( 13.39449014422897122, 13.16814630638014272, 5.497670784391714527 ) ) ;
#3561 = CARTESIAN_POINT ( 'NONE',  ( 6.815620469402779769, 10.91373323652594252, 4.223291697927726851 ) ) ;
#3562 = CARTESIAN_POINT ( 'NONE',  ( -0.1849527129589544072, 21.03045532914853055, 5.150944214860931680 ) ) ;
#3563 = EDGE_CURVE ( 'NONE', #15983, #1266, #4052, .T. ) ;
#3564 = EDGE_CURVE ( 'NONE', #14025, #8219, #17865, .T. ) ;
#3565 = CARTESIAN_POINT ( 'NONE',  ( 30.25543876212147509, 32.54502000000000095, -19.39939755251907272 ) ) ;
#3566 = CARTESIAN_POINT ( 'NONE',  ( 0.1086559561431187093, 17.19705222221691088, 0.7960978371211332449 ) ) ;
#3567 = DIRECTION ( 'NONE',  ( 0.8609107660235849613, 0.000000000000000000, -0.5087559856598092844 ) ) ;
#3568 = DIRECTION ( 'NONE',  ( 0.08420877549337300871, 0.000000000000000000, 0.9964481331860212121 ) ) ;
#3569 = CARTESIAN_POINT ( 'NONE',  ( 10.77029199848827368, -2.261732460827042157, -17.08557667898591603 ) ) ;
#3570 = AXIS2_PLACEMENT_3D ( 'NONE', #13020, #19952, #4600 ) ;
#3571 = CARTESIAN_POINT ( 'NONE',  ( 13.86631606410951534, 16.88209101360638797, -18.21726315170741017 ) ) ;
#3572 = VECTOR ( 'NONE', #2942, 1000.000000000000000 ) ;
#3573 = VECTOR ( 'NONE', #19065, 1000.000000000000000 ) ;
#3574 = CARTESIAN_POINT ( 'NONE',  ( 11.41259685292655668, 16.31337187110278464, 7.583935353899422083 ) ) ;
#3575 = DIRECTION ( 'NONE',  ( 0.7421532822901579785, 0.000000000000000000, -0.6702301885068628895 ) ) ;
#3576 = ORIENTED_EDGE ( 'NONE', *, *, #15564, .T. ) ;
#3577 = CARTESIAN_POINT ( 'NONE',  ( 13.08605924474404425, 16.89445423263737567, 6.385784896790035248 ) ) ;
#3578 = DIRECTION ( 'NONE',  ( 0.000000000000000000, -1.000000000000000000, -0.000000000000000000 ) ) ;
#3579 = CARTESIAN_POINT ( 'NONE',  ( 2.134098633783316323, 19.31779869980666220, 1.050363145643365748 ) ) ;
#3580 = ORIENTED_EDGE ( 'NONE', *, *, #21423, .T. ) ;
#3581 = CARTESIAN_POINT ( 'NONE',  ( -7.949728765565600597, -0.7997824999999986195, -34.47798802950714503 ) ) ;
#3582 = CARTESIAN_POINT ( 'NONE',  ( 4.871060933462843856, 20.35131442480351183, 1.748582030751478111 ) ) ;
#3583 = DIRECTION ( 'NONE',  ( 0.000000000000000000, 0.000000000000000000, 1.000000000000000000 ) ) ;
#3584 = CARTESIAN_POINT ( 'NONE',  ( 50.29383871662588490, -1.983739999999999837, -28.02957329025317179 ) ) ;
#3585 = ADVANCED_FACE ( 'NONE', ( #18487 ), #20127, .F. ) ;
#3586 = AXIS2_PLACEMENT_3D ( 'NONE', #2532, #16041, #17571 ) ;
#3587 = EDGE_CURVE ( 'NONE', #15164, #1238, #6869, .T. ) ;
#3588 = AXIS2_PLACEMENT_3D ( 'NONE', #12638, #19470, #21126 ) ;
#3589 = EDGE_CURVE ( 'NONE', #16780, #8026, #3789, .T. ) ;
#3590 = VERTEX_POINT ( 'NONE', #3360 ) ;
#3591 = CARTESIAN_POINT ( 'NONE',  ( 11.22303388661927137, 15.74982258328167717, 6.891629373590611785 ) ) ;
#3592 = CARTESIAN_POINT ( 'NONE',  ( 12.27006042634966931, 20.89186537925146325, -1.183231535759053710 ) ) ;
#3593 = CARTESIAN_POINT ( 'NONE',  ( 4.880215608511783820, 20.21972024448168170, 0.5016143470315571617 ) ) ;
#3594 = CARTESIAN_POINT ( 'NONE',  ( 11.14637220089711001, 12.02381550237932295, 5.878899239644039376 ) ) ;
#3595 = CIRCLE ( 'NONE', #21595, 0.7950199999999993938 ) ;
#3596 = PLANE ( 'NONE',  #16758 ) ;
#3597 = CARTESIAN_POINT ( 'NONE',  ( 17.98289846892998156, -6.707016923903890593, -15.66823201329469661 ) ) ;
#3598 = DIRECTION ( 'NONE',  ( 0.000000000000000000, 1.000000000000000000, -0.000000000000000000 ) ) ;
#3599 = EDGE_LOOP ( 'NONE', ( #7691, #17588, #10865, #20840 ) ) ;
#3600 = CARTESIAN_POINT ( 'NONE',  ( 7.570358912651840910, 21.81389254086020202, 3.244435738127268376 ) ) ;
#3601 = VECTOR ( 'NONE', #17795, 1000.000000000000000 ) ;
#3602 = ORIENTED_EDGE ( 'NONE', *, *, #7776, .T. ) ;
#3603 = AXIS2_PLACEMENT_3D ( 'NONE', #6066, #3514, #3409 ) ;
#3604 = AXIS2_PLACEMENT_3D ( 'NONE', #13602, #15378, #3964 ) ;
#3605 = DIRECTION ( 'NONE',  ( 0.000000000000000000, 1.000000000000000000, 0.000000000000000000 ) ) ;
#3606 = DIRECTION ( 'NONE',  ( -1.000000000000000000, 0.000000000000000000, 0.000000000000000000 ) ) ;
#3608 = CARTESIAN_POINT ( 'NONE',  ( 21.03437500000000071, 32.54502000000000095, 5.159374999999999822 ) ) ;
#3607 = CARTESIAN_POINT ( 'NONE',  ( 3.634833444273914083, 19.07995194538682071, -0.6453590074123158882 ) ) ;
#3609 = EDGE_LOOP ( 'NONE', ( #3549, #3366, #2243, #17336 ) ) ;
#3610 = CARTESIAN_POINT ( 'NONE',  ( 7.548729492735156477, 15.22146907589735676, 8.284681895849521638 ) ) ;
#3611 = AXIS2_PLACEMENT_3D ( 'NONE', #9381, #976, #7726 ) ;
#3612 = DIRECTION ( 'NONE',  ( 0.9579671649362034858, 0.000000000000000000, -0.2868778675745011220 ) ) ;
#3613 = ORIENTED_EDGE ( 'NONE', *, *, #12901, .F. ) ;
#3614 = VECTOR ( 'NONE', #20424, 1000.000000000000000 ) ;
#3615 = EDGE_CURVE ( 'NONE', #12583, #4819, #18589, .T. ) ;
#3616 = ADVANCED_FACE ( 'NONE', ( #5114 ), #6144, .T. ) ;
#3617 = CARTESIAN_POINT ( 'NONE',  ( -47.86112874365709047, 38.26001999999999725, -23.29368419115692035 ) ) ;
#3618 = ORIENTED_EDGE ( 'NONE', *, *, #20772, .T. ) ;
#3619 = AXIS2_PLACEMENT_3D ( 'NONE', #9653, #19702, #13319 ) ;
#3620 = CARTESIAN_POINT ( 'NONE',  ( 12.88040283537677588, 12.29391749999999739, -0.09070320285213756550 ) ) ;
#3621 = CARTESIAN_POINT ( 'NONE',  ( 1.998220421679061776, 34.04486736277070236, -22.64748046904500356 ) ) ;
#3622 = DIRECTION ( 'NONE',  ( 0.8741107132214044340, 0.000000000000000000, 0.4857267349359799535 ) ) ;
#3623 = VECTOR ( 'NONE', #3606, 1000.000000000000000 ) ;
#3624 = LINE ( 'NONE', #13805, #21432 ) ;
#3625 = CIRCLE ( 'NONE', #7165, 0.5080000000000023386 ) ;
#3626 = ORIENTED_EDGE ( 'NONE', *, *, #7995, .T. ) ;
#3627 = CYLINDRICAL_SURFACE ( 'NONE', #12472, 3.968750000000000000 ) ;
#3628 = DIRECTION ( 'NONE',  ( 0.000000000000000000, 0.000000000000000000, -1.000000000000000000 ) ) ;
#3629 = LINE ( 'NONE', #10476, #3187 ) ;
#3631 = CARTESIAN_POINT ( 'NONE',  ( 11.99812378058872930, -4.884789211543026255, -15.65751131229454352 ) ) ;
#3630 = DIRECTION ( 'NONE',  ( 0.000000000000000000, 1.000000000000000000, 0.000000000000000000 ) ) ;
#3632 = ORIENTED_EDGE ( 'NONE', *, *, #15903, .T. ) ;
#3633 = ORIENTED_EDGE ( 'NONE', *, *, #21383, .F. ) ;
#3634 = CARTESIAN_POINT ( 'NONE',  ( 10.92369501690972200, 12.61980174807018251, 5.367099221840908818 ) ) ;
#3635 = CARTESIAN_POINT ( 'NONE',  ( -0.1924500159166692703, 15.59650202059448354, -0.009168507438969686341 ) ) ;
#3636 = ORIENTED_EDGE ( 'NONE', *, *, #13339, .F. ) ;
#3637 = AXIS2_PLACEMENT_3D ( 'NONE', #15254, #6832, #21756 ) ;
#3638 = ORIENTED_EDGE ( 'NONE', *, *, #11278, .T. ) ;
#3639 = LINE ( 'NONE', #6946, #13108 ) ;
#3640 = ORIENTED_EDGE ( 'NONE', *, *, #14297, .T. ) ;
#3641 = CARTESIAN_POINT ( 'NONE',  ( 7.519266203142771943, 13.69322247944533189, -1.339971849629911782 ) ) ;
#3642 = EDGE_CURVE ( 'NONE', #20985, #1632, #11500, .T. ) ;
#3643 = AXIS2_PLACEMENT_3D ( 'NONE', #12774, #18270, #3128 ) ;
#3644 = ORIENTED_EDGE ( 'NONE', *, *, #13978, .F. ) ;
#3645 = CARTESIAN_POINT ( 'NONE',  ( -23.01875000000000071, 32.54502000000000095, -3.968750000000000000 ) ) ;
#3646 = VECTOR ( 'NONE', #5382, 1000.000000000000000 ) ;
#3647 = LINE ( 'NONE', #16707, #5422 ) ;
#3648 = LINE ( 'NONE', #1753, #20606 ) ;
#3649 = CYLINDRICAL_SURFACE ( 'NONE', #4762, 3.970020000000001215 ) ;
#3650 = CARTESIAN_POINT ( 'NONE',  ( 2.344389418299225980, 20.87639896374770032, 6.272429502486324360 ) ) ;
#3651 = ORIENTED_EDGE ( 'NONE', *, *, #14153, .T. ) ;
#3652 = CARTESIAN_POINT ( 'NONE',  ( 2.174318833424090602, 16.42212273390128985, -0.1944002137027950050 ) ) ;
#3653 = CARTESIAN_POINT ( 'NONE',  ( 22.04181838752732148, 16.26393749999999727, 0.06645525512612464325 ) ) ;
#3654 = DIRECTION ( 'NONE',  ( 0.000000000000000000, 1.000000000000000000, 0.000000000000000000 ) ) ;
#3655 = CARTESIAN_POINT ( 'NONE',  ( 53.84486179190094646, 32.54502000000000095, -6.412645463410259872 ) ) ;
#3656 = ORIENTED_EDGE ( 'NONE', *, *, #15060, .T. ) ;
#3657 = CARTESIAN_POINT ( 'NONE',  ( 11.03612856729982816, 18.39344551543849704, -4.120841951098963563 ) ) ;
#3658 = AXIS2_PLACEMENT_3D ( 'NONE', #3077, #9800, #8144 ) ;
#3659 = DIRECTION ( 'NONE',  ( 0.000000000000000000, -1.000000000000000000, 0.000000000000000000 ) ) ;
#3660 = CARTESIAN_POINT ( 'NONE',  ( 13.07567957613725618, 18.69954703227123716, 6.688832392068873034 ) ) ;
#3661 = ORIENTED_EDGE ( 'NONE', *, *, #9023, .F. ) ;
#3662 = FACE_OUTER_BOUND ( 'NONE', #2631, .T. ) ;
#3663 = ORIENTED_EDGE ( 'NONE', *, *, #18069, .T. ) ;
#3664 = CARTESIAN_POINT ( 'NONE',  ( 14.25617145423489696, 36.51313500000000545, -15.80779474975094168 ) ) ;
#3665 = CARTESIAN_POINT ( 'NONE',  ( 9.494052425882697932, 15.50413968533264963, 7.929839997388628881 ) ) ;
#3666 = CARTESIAN_POINT ( 'NONE',  ( -0.6181405386100876642, 20.05178378372840342, 3.961315155216848183 ) ) ;
#3667 = CYLINDRICAL_SURFACE ( 'NONE', #13017, 0.5080000000000007843 ) ;
#3668 = CARTESIAN_POINT ( 'NONE',  ( 5.899279335236281341, 18.34365586212437549, -0.9761941005625609513 ) ) ;
#3669 = VECTOR ( 'NONE', #3531, 1000.000000000000000 ) ;
#3670 = EDGE_CURVE ( 'NONE', #20634, #14970, #10774, .T. ) ;
#3671 = CARTESIAN_POINT ( 'NONE',  ( 1.286080621724394302, 20.22460181342998098, 3.469449174071038922 ) ) ;
#3672 = CARTESIAN_POINT ( 'NONE',  ( 38.99879864891609316, 37.69823060749433807, -3.901399344704656436 ) ) ;
#3673 = CARTESIAN_POINT ( 'NONE',  ( 9.335363283976800375, -3.968114999999999615, -14.20581391854862474 ) ) ;
#3674 = CARTESIAN_POINT ( 'NONE',  ( 6.093765842861319726, 19.19176664446208136, -1.521969077160680861 ) ) ;
#3675 = VECTOR ( 'NONE', #3945, 1000.000000000000000 ) ;
#3676 = CARTESIAN_POINT ( 'NONE',  ( 0.7454037288853153642, 11.31615121391088152, 4.862722110801131592 ) ) ;
#3677 = CARTESIAN_POINT ( 'NONE',  ( -17.46249999999999858, 0.000000000000000000, 0.000000000000000000 ) ) ;
#3678 = CARTESIAN_POINT ( 'NONE',  ( 20.19361157104201965, -1.031857205123764887, -14.76988187127798113 ) ) ;
#3679 = DIRECTION ( 'NONE',  ( 0.000000000000000000, 1.000000000000000000, 0.000000000000000000 ) ) ;
#3680 = DIRECTION ( 'NONE',  ( 0.000000000000000000, 1.000000000000000000, 0.000000000000000000 ) ) ;
#3681 = CARTESIAN_POINT ( 'NONE',  ( 14.52649824764486652, -8.218679500498163648, -16.40164373686755184 ) ) ;
#3682 = FACE_OUTER_BOUND ( 'NONE', #6468, .T. ) ;
#3683 = CARTESIAN_POINT ( 'NONE',  ( 28.56548256563643662, 36.51313500000000545, -12.12873025803960658 ) ) ;
#3684 = CARTESIAN_POINT ( 'NONE',  ( 9.028135976095729376, 21.80991532760212337, 1.508259505891954344 ) ) ;
#3685 = ADVANCED_FACE ( 'NONE', ( #7967, #12965, #16709 ), #14513, .F. ) ;
#3686 = CARTESIAN_POINT ( 'NONE',  ( 9.335363283976800375, -1.983739999999999393, -14.20581391854862474 ) ) ;
#3687 = FACE_OUTER_BOUND ( 'NONE', #4070, .T. ) ;
#3688 = CARTESIAN_POINT ( 'NONE',  ( 11.18059225887507324, 16.35212281796569656, -3.590113610534638067 ) ) ;
#3689 = CARTESIAN_POINT ( 'NONE',  ( 14.58173340751025471, -7.269924891899197661, -16.42976176385494469 ) ) ;
#3691 = DIRECTION ( 'NONE',  ( -0.8667647648559581031, 0.000000000000000000, -0.4987171968201974948 ) ) ;
#3690 = CARTESIAN_POINT ( 'NONE',  ( 1.780830151919097659, 17.97529088148248277, 0.2652343077119106995 ) ) ;
#3692 = CIRCLE ( 'NONE', #1221, 0.5953125000000005773 ) ;
#3693 = ORIENTED_EDGE ( 'NONE', *, *, #14369, .T. ) ;
#3694 = SHAPE_DEFINITION_REPRESENTATION ( #2425, #10883 ) ;
#3695 = CARTESIAN_POINT ( 'NONE',  ( 2.063750000000000195, 30.56064500000000095, 8.335010000000000474 ) ) ;
#3696 = EDGE_CURVE ( 'NONE', #13654, #13907, #13968, .T. ) ;
#3697 = EDGE_CURVE ( 'NONE', #6074, #18112, #14957, .T. ) ;
#3698 = ADVANCED_FACE ( 'NONE', ( #5087 ), #18779, .F. ) ;
#3699 = CARTESIAN_POINT ( 'NONE',  ( 6.323699694823708306, 11.70956187560891237, 2.868955871455586948 ) ) ;
#3700 = VECTOR ( 'NONE', #3679, 1000.000000000000000 ) ;
#3701 = ORIENTED_EDGE ( 'NONE', *, *, #19264, .T. ) ;
#3702 = CARTESIAN_POINT ( 'NONE',  ( 10.28015363549983263, 20.34374524028692122, 4.926689491331847748 ) ) ;
#3703 = CARTESIAN_POINT ( 'NONE',  ( 8.215498187051487378, 11.48837196139402295, 1.847920089096604102 ) ) ;
#3704 = CARTESIAN_POINT ( 'NONE',  ( 6.457449847458724967, 11.64278443974904320, 1.165535279167791316 ) ) ;
#3705 = CARTESIAN_POINT ( 'NONE',  ( 7.525827410530302686, 21.81319771123894213, 3.257719107942246950 ) ) ;
#3706 = CARTESIAN_POINT ( 'NONE',  ( 49.81956284419040060, 32.54502000000000095, 11.98436472153758103 ) ) ;
#3707 = CARTESIAN_POINT ( 'NONE',  ( 17.15392603081281564, 0.8698987389447586649, -15.10081136307826988 ) ) ;
#3708 = LINE ( 'NONE', #6802, #5999 ) ;
#3709 = ORIENTED_EDGE ( 'NONE', *, *, #17974, .T. ) ;
#3710 = CARTESIAN_POINT ( 'NONE',  ( 8.647929108115961938, 10.74346438930206027, 3.686466043081342736 ) ) ;
#3711 = ADVANCED_FACE ( 'NONE', ( #13391 ), #21881, .F. ) ;
#3712 = CIRCLE ( 'NONE', #17850, 0.7950200000000000600 ) ;
#3713 = ORIENTED_EDGE ( 'NONE', *, *, #20042, .F. ) ;
#3714 = CARTESIAN_POINT ( 'NONE',  ( 9.303952506480500872, 14.60406769983332076, -2.545567318552978353 ) ) ;
#3715 = PRODUCT_DEFINITION ( 'UNKNOWN', '', #12664, #10552 ) ;
#3716 = DIRECTION ( 'NONE',  ( -0.2490110332224850231, 0.000000000000000000, 0.9685006480810791629 ) ) ;
#3717 = CARTESIAN_POINT ( 'NONE',  ( 12.75852270247490949, 22.12259436858274242, 0.1659619235736507770 ) ) ;
#3719 = LINE ( 'NONE', #15347, #6394 ) ;
#3718 = CARTESIAN_POINT ( 'NONE',  ( 6.533579059798534594, 20.03265763155913959, 7.061703031544717568 ) ) ;
#3720 = ORIENTED_EDGE ( 'NONE', *, *, #14274, .T. ) ;
#3721 =( LENGTH_UNIT ( ) NAMED_UNIT ( * ) SI_UNIT ( .MILLI., .METRE. ) );
#3722 = EDGE_CURVE ( 'NONE', #8462, #9830, #12907, .T. ) ;
#3723 = CARTESIAN_POINT ( 'NONE',  ( -157.1365884395040098, 9.924415000000001541, 46.81779025872040023 ) ) ;
#3724 = EDGE_LOOP ( 'NONE', ( #10788, #16458, #5932, #4732, #974, #10027 ) ) ;
#3725 = EDGE_CURVE ( 'NONE', #19311, #7286, #16807, .T. ) ;
#3726 = EDGE_CURVE ( 'NONE', #21188, #16869, #19921, .T. ) ;
#3727 = CARTESIAN_POINT ( 'NONE',  ( 0.04319471458505506206, 15.89914589079416807, 0.8258939165814165317 ) ) ;
#3728 = DIRECTION ( 'NONE',  ( 0.000000000000000000, 1.000000000000000000, 0.000000000000000000 ) ) ;
#3729 = ORIENTED_EDGE ( 'NONE', *, *, #16884, .T. ) ;
#3730 = AXIS2_PLACEMENT_3D ( 'NONE', #17397, #8745, #10527 ) ;
#3731 = CARTESIAN_POINT ( 'NONE',  ( 3.733140608333783916, 15.17434541625935651, -0.5071927740268031837 ) ) ;
#3732 = DIRECTION ( 'NONE',  ( 0.9999999998269335499, -1.860465115920061245E-05, 0.000000000000000000 ) ) ;
#3733 = DIRECTION ( 'NONE',  ( -0.7421532822901579785, 0.000000000000000000, 0.6702301885068630005 ) ) ;
#3734 = DIRECTION ( 'NONE',  ( 0.9579671649362032637, 0.000000000000000000, -0.2868778675745013440 ) ) ;
#3735 = CARTESIAN_POINT ( 'NONE',  ( 3.370024690280242208, 21.31626652883829465, 3.345821271410136077 ) ) ;
#3736 = DIRECTION ( 'NONE',  ( 0.9784543669157820256, 0.000000000000000000, 0.2064631973583577473 ) ) ;
#3737 = VERTEX_POINT ( 'NONE', #15389 ) ;
#3738 = FACE_OUTER_BOUND ( 'NONE', #18756, .T. ) ;
#3739 = DIRECTION ( 'NONE',  ( -0.9685006480810792739, 0.000000000000000000, -0.2490110332224846346 ) ) ;
#3740 = CYLINDRICAL_SURFACE ( 'NONE', #19491, 9.524999999999998579 ) ;
#3741 = EDGE_CURVE ( 'NONE', #9035, #9720, #10496, .T. ) ;
#3743 = CARTESIAN_POINT ( 'NONE',  ( 11.89701557769404339, -4.657576675299070601, -15.67185707629564106 ) ) ;
#3742 = CARTESIAN_POINT ( 'NONE',  ( -2.028188046367890074, 9.129395000000000593, 0.3682158094503220069 ) ) ;
#3744 = ORIENTED_EDGE ( 'NONE', *, *, #20410, .T. ) ;
#3745 = ADVANCED_FACE ( 'NONE', ( #6955 ), #11934, .T. ) ;
#3746 = ORIENTED_EDGE ( 'NONE', *, *, #18516, .F. ) ;
#3747 = ADVANCED_FACE ( 'NONE', ( #12166 ), #3649, .T. ) ;
#3748 = CARTESIAN_POINT ( 'NONE',  ( 12.16242873554583959, 20.88809130931168312, -1.148875002998984041 ) ) ;
#3750 = DIRECTION ( 'NONE',  ( -0.1060008583745199739, 0.000000000000000000, -0.9943660382494290406 ) ) ;
#3749 = CARTESIAN_POINT ( 'NONE',  ( 3.938429258113647968, 19.12622466589174053, -0.8127979641362345076 ) ) ;
#3751 = ORIENTED_EDGE ( 'NONE', *, *, #18097, .F. ) ;
#3752 = CARTESIAN_POINT ( 'NONE',  ( 4.648553867220805991, 11.09625097007389094, 4.080894491436514393 ) ) ;
#3753 = ORIENTED_EDGE ( 'NONE', *, *, #758, .F. ) ;
#3754 = ORIENTED_EDGE ( 'NONE', *, *, #18480, .T. ) ;
#3755 = CARTESIAN_POINT ( 'NONE',  ( 7.796429656384849416, 12.28811609040251085, 0.04948816907226474826 ) ) ;
#3756 = ORIENTED_EDGE ( 'NONE', *, *, #17014, .T. ) ;
#3757 = CARTESIAN_POINT ( 'NONE',  ( 3.338557919237726601, 13.67037593795628148, 7.539146506506522627 ) ) ;
#3758 = CARTESIAN_POINT ( 'NONE',  ( 52.49113927203449492, -6.356984999999999886, -16.14695822742181619 ) ) ;
#3759 = LINE ( 'NONE', #17572, #21311 ) ;
#3760 = CARTESIAN_POINT ( 'NONE',  ( 54.55586098912687731, -9.531985000000000596, -6.056925149195119040 ) ) ;
#3761 = FACE_OUTER_BOUND ( 'NONE', #9032, .T. ) ;
#3762 = CARTESIAN_POINT ( 'NONE',  ( 2.520972058354161049, 20.65036714207981206, 6.740181459500954375 ) ) ;
#3763 = DIRECTION ( 'NONE',  ( 0.1060008583745224581, 0.000000000000000000, 0.9943660382494288186 ) ) ;
#3764 = ORIENTED_EDGE ( 'NONE', *, *, #2696, .F. ) ;
#3765 = CARTESIAN_POINT ( 'NONE',  ( 0.8347132962655614552, 12.00400186595892293, 3.168484099998905901 ) ) ;
#3766 = DIRECTION ( 'NONE',  ( 0.000000000000000000, -1.000000000000000000, -0.000000000000000000 ) ) ;
#3767 = CARTESIAN_POINT ( 'NONE',  ( 52.36707797519913044, -5.757307957063426684, -17.43673301238325379 ) ) ;
#3768 = DIRECTION ( 'NONE',  ( 0.000000000000000000, 1.000000000000000000, 0.000000000000000000 ) ) ;
#3769 = FACE_OUTER_BOUND ( 'NONE', #14793, .T. ) ;
#3770 = VERTEX_POINT ( 'NONE', #18890 ) ;
#3771 = EDGE_CURVE ( 'NONE', #1261, #12179, #18194, .T. ) ;
#3772 = CARTESIAN_POINT ( 'NONE',  ( 9.192284307488497674, 19.28339334790884152, -2.815733911810373247 ) ) ;
#3773 = DIRECTION ( 'NONE',  ( -0.8609107660235850723, 0.000000000000000000, 0.5087559856598092844 ) ) ;
#3774 = CARTESIAN_POINT ( 'NONE',  ( 11.90889849114380716, 21.69093323893340397, 3.651447091914156395 ) ) ;
#3775 = ORIENTED_EDGE ( 'NONE', *, *, #12412, .T. ) ;
#3776 = ORIENTED_EDGE ( 'NONE', *, *, #7706, .T. ) ;
#3777 = LINE ( 'NONE', #13852, #14159 ) ;
#3778 = CARTESIAN_POINT ( 'NONE',  ( 9.496579142445281008, 15.25906563848011110, 7.888626892806992252 ) ) ;
#3779 = CARTESIAN_POINT ( 'NONE',  ( -0.2797058817397305996, 20.30753595452681992, 4.828421465540532864 ) ) ;
#3780 = CARTESIAN_POINT ( 'NONE',  ( 29.64606458365116737, -6.752907499999998286, -15.53894806404596096 ) ) ;
#3781 = CARTESIAN_POINT ( 'NONE',  ( 6.212096097470904965, 11.84283872956120121, 2.029147759238299376 ) ) ;
#3782 = CARTESIAN_POINT ( 'NONE',  ( -15.71080452296940599, -14.84248999999999974, -10.47737680862620380 ) ) ;
#3783 = FACE_OUTER_BOUND ( 'NONE', #21030, .T. ) ;
#3784 = AXIS2_PLACEMENT_3D ( 'NONE', #11766, #8422, #6990 ) ;
#3785 = CARTESIAN_POINT ( 'NONE',  ( 9.500433685271497453, 18.52979832374122182, 7.486654841140969907 ) ) ;
#3786 = CARTESIAN_POINT ( 'NONE',  ( 0.6580577011572460444, 20.32439072914841915, 1.809299870180519632 ) ) ;
#3787 = CARTESIAN_POINT ( 'NONE',  ( 0.7837585588936004655, 20.18907768623580878, 7.715511287553819209 ) ) ;
#3788 = DIRECTION ( 'NONE',  ( 0.1060008583745200711, 0.000000000000000000, 0.9943660382494290406 ) ) ;
#3789 = LINE ( 'NONE', #18698, #17107 ) ;
#3790 = LINE ( 'NONE', #19147, #17678 ) ;
#3791 = CARTESIAN_POINT ( 'NONE',  ( 64.66604708500285881, 0.000000000000000000, -11.54913207920052720 ) ) ;
#3792 = CARTESIAN_POINT ( 'NONE',  ( 15.20375925029796349, 2.251092030198116323, -15.69209066710536682 ) ) ;
#3793 = DIRECTION ( 'NONE',  ( 0.000000000000000000, -1.000000000000000000, -0.000000000000000000 ) ) ;
#3794 = EDGE_CURVE ( 'NONE', #1425, #10463, #20099, .T. ) ;
#3795 = CARTESIAN_POINT ( 'NONE',  ( 32.42378190387104553, 32.54502000000000095, -18.15178106273469183 ) ) ;
#3796 = CARTESIAN_POINT ( 'NONE',  ( 10.90717967712175351, 19.59065766869934322, 6.581256167405926227 ) ) ;
#3797 = CARTESIAN_POINT ( 'NONE',  ( 30.41963056417667488, 34.52875999999999834, -8.653862521447852174 ) ) ;
#3798 = CARTESIAN_POINT ( 'NONE',  ( 11.16427926597950915, 16.07250702038418311, -3.584404996504540364 ) ) ;
#3799 = VECTOR ( 'NONE', #11020, 1000.000000000000000 ) ;
#3800 = DIRECTION ( 'NONE',  ( 0.000000000000000000, 1.000000000000000000, 0.000000000000000000 ) ) ;
#3801 = CARTESIAN_POINT ( 'NONE',  ( 1.004559003390568472, 18.49730447209151762, 8.359447931242584673 ) ) ;
#3802 = ORIENTED_EDGE ( 'NONE', *, *, #4272, .T. ) ;
#3803 = SHAPE_DEFINITION_REPRESENTATION ( #19043, #17083 ) ;
#3804 = CARTESIAN_POINT ( 'NONE',  ( 1.173720826352361080, -1.594802499999999013, -20.82884779549221577 ) ) ;
#3805 = CARTESIAN_POINT ( 'NONE',  ( 4.409735924645852734, 19.51568168759821020, 0.5807916733966671519 ) ) ;
#3806 = CARTESIAN_POINT ( 'NONE',  ( 29.01020070778135818, -14.84248999999999974, -13.85841188422236492 ) ) ;
#3807 = ORIENTED_EDGE ( 'NONE', *, *, #2624, .T. ) ;
#3808 = CARTESIAN_POINT ( 'NONE',  ( 7.513641844582591212, 14.65140826333467139, -1.943504412708490614 ) ) ;
#3809 = CARTESIAN_POINT ( 'NONE',  ( 4.288245895386477713, 20.16661322485262531, 5.765686568166492165 ) ) ;
#3810 = CARTESIAN_POINT ( 'NONE',  ( 10.72173680743496149, 11.64719608603622270, 3.872061749179875001 ) ) ;
#3811 = CARTESIAN_POINT ( 'NONE',  ( 5.387809698622330501, 11.72601213311298274, 5.352900495692114902 ) ) ;
#3812 = CARTESIAN_POINT ( 'NONE',  ( 11.10116566411557137, 18.39169315105245417, -4.135447224377957198 ) ) ;
#3813 = VECTOR ( 'NONE', #4286, 1000.000000000000000 ) ;
#3814 = CARTESIAN_POINT ( 'NONE',  ( 53.10651001381376091, -7.547610000000002373, -16.70269254552787075 ) ) ;
#3815 = CARTESIAN_POINT ( 'NONE',  ( 19.16641761350585327, -0.7858219696195261061, -14.45522876183969885 ) ) ;
#3816 = CARTESIAN_POINT ( 'NONE',  ( 31.75000000000000000, 32.54502000000000095, -4.317999999999999616 ) ) ;
#3817 = ADVANCED_FACE ( 'NONE', ( #20314 ), #10060, .T. ) ;
#3818 = ORIENTED_EDGE ( 'NONE', *, *, #1115, .F. ) ;
#3819 = ADVANCED_FACE ( 'NONE', ( #20213 ), #104, .F. ) ;
#3820 = CARTESIAN_POINT ( 'NONE',  ( 11.06727400676183670, 17.45221349387399812, 6.693287419277384132 ) ) ;
#3821 = CARTESIAN_POINT ( 'NONE',  ( 11.56876908001934900, 20.24893436370382105, -3.130508153246869263 ) ) ;
#3822 = CARTESIAN_POINT ( 'NONE',  ( 53.08681243024872742, 40.07829845791615497, -16.72443647849243575 ) ) ;
#3823 = ORIENTED_EDGE ( 'NONE', *, *, #13613, .T. ) ;
#3824 = CARTESIAN_POINT ( 'NONE',  ( 9.490928692825109536, 12.85459832499831201, -1.457268345192402226 ) ) ;
#3825 = DIRECTION ( 'NONE',  ( 0.000000000000000000, 1.000000000000000000, 0.000000000000000000 ) ) ;
#3826 = CARTESIAN_POINT ( 'NONE',  ( 29.83577936850046441, 16.26393749999999727, -2.267565145593293696 ) ) ;
#3828 = CARTESIAN_POINT ( 'NONE',  ( 64.19677489640052670, -1.983739999999999837, -11.74367670905533423 ) ) ;
#3827 = CARTESIAN_POINT ( 'NONE',  ( -1.187794103216660790, 20.48604666719226230, 3.371823117913468337 ) ) ;
#3829 = EDGE_LOOP ( 'NONE', ( #4200, #14448, #19212, #13377, #10019 ) ) ;
#3830 = CARTESIAN_POINT ( 'NONE',  ( 7.367551414186734426, 12.78932470803417765, 7.116237235135340455 ) ) ;
#3831 = DIRECTION ( 'NONE',  ( 0.2490110332224850231, 0.000000000000000000, -0.9685006480810791629 ) ) ;
#3832 = CIRCLE ( 'NONE', #14786, 0.7950200000000003930 ) ;
#3833 = VERTEX_POINT ( 'NONE', #216 ) ;
#3834 = CARTESIAN_POINT ( 'NONE',  ( 38.96848998618624904, 40.07865999999999929, -3.934807454472129429 ) ) ;
#3835 = CARTESIAN_POINT ( 'NONE',  ( -4.157227781567939928, 9.924415000000001541, 0.1758860224507720060 ) ) ;
#3836 = ORIENTED_EDGE ( 'NONE', *, *, #3946, .F. ) ;
#3837 = DIRECTION ( 'NONE',  ( -0.9724402360367336851, 0.000000000000000000, 0.2331522835762537549 ) ) ;
#3838 = CARTESIAN_POINT ( 'NONE',  ( 1.881385393434782394, 15.19240802041391802, 0.2309439307633842919 ) ) ;
#3839 = ADVANCED_FACE ( 'NONE', ( #3761 ), #1547, .T. ) ;
#3840 = LINE ( 'NONE', #20504, #12824 ) ;
#3841 = CARTESIAN_POINT ( 'NONE',  ( 12.13621795668766445, 34.52875999999999834, 4.225309685850866082 ) ) ;
#3842 = DIRECTION ( 'NONE',  ( 0.2868778675745011220, 0.000000000000000000, 0.9579671649362034858 ) ) ;
#3843 = CARTESIAN_POINT ( 'NONE',  ( 1.883505690267595956, 8.857556300445232011, 10.71562500000000107 ) ) ;
#3844 = VECTOR ( 'NONE', #13436, 1000.000000000000000 ) ;
#3845 = VERTEX_POINT ( 'NONE', #10392 ) ;
#3846 = EDGE_CURVE ( 'NONE', #17811, #1768, #21346, .T. ) ;
#3847 = CARTESIAN_POINT ( 'NONE',  ( -21.45091887247874851, 40.79338547039380103, -9.992285829511605044 ) ) ;
#3848 = CARTESIAN_POINT ( 'NONE',  ( 61.04701390398659555, 34.52875999999999834, -15.15157976445104993 ) ) ;
#3850 = CARTESIAN_POINT ( 'NONE',  ( 17.27833917726472635, -6.912512178730144008, -14.59757655905045937 ) ) ;
#3849 = CARTESIAN_POINT ( 'NONE',  ( -1.351150467732365579, 2.373947500000000765, -27.17319717629097653 ) ) ;
#3851 = ORIENTED_EDGE ( 'NONE', *, *, #1681, .F. ) ;
#3852 = ORIENTED_EDGE ( 'NONE', *, *, #18929, .F. ) ;
#3853 = CARTESIAN_POINT ( 'NONE',  ( 11.91509809843844003, 11.13638386089868249, 0.7869662318407120161 ) ) ;
#3855 = CARTESIAN_POINT ( 'NONE',  ( 48.58367710892853353, -1.983739999999999837, -25.32442392637788231 ) ) ;
#3854 = CARTESIAN_POINT ( 'NONE',  ( 3.508358100546943525, 15.44872671029758671, -1.459857323000175899 ) ) ;
#3856 = VERTEX_POINT ( 'NONE', #21774 ) ;
#3858 = CARTESIAN_POINT ( 'NONE',  ( 17.28797397335993935, 2.432764323952259389, -15.11463947043034040 ) ) ;
#3857 = CARTESIAN_POINT ( 'NONE',  ( 5.598674578815908909, 15.44076680689341607, 8.728037113477167708 ) ) ;
#3859 = AXIS2_PLACEMENT_3D ( 'NONE', #16184, #17331, #8801 ) ;
#3860 = ADVANCED_FACE ( 'NONE', ( #2310 ), #9266, .F. ) ;
#3861 = ORIENTED_EDGE ( 'NONE', *, *, #15671, .F. ) ;
#3862 = ORIENTED_EDGE ( 'NONE', *, *, #5153, .T. ) ;
#3863 = CARTESIAN_POINT ( 'NONE',  ( 8.009488492024781081, 19.38248615295674426, -1.109337938200560369 ) ) ;
#3864 = ORIENTED_EDGE ( 'NONE', *, *, #10321, .T. ) ;
#3865 = CARTESIAN_POINT ( 'NONE',  ( 3.400495240568472077, 16.13495438657706771, 8.445061970360232095 ) ) ;
#3866 = ADVANCED_FACE ( 'NONE', ( #14377 ), #20996, .T. ) ;
#3867 = EDGE_CURVE ( 'NONE', #8700, #18216, #8288, .T. ) ;
#3868 = VECTOR ( 'NONE', #3716, 1000.000000000000114 ) ;
#3869 = EDGE_CURVE ( 'NONE', #18216, #6968, #7191, .T. ) ;
#3870 = CARTESIAN_POINT ( 'NONE',  ( -51.02421882195815783, -5.714364999999999029, -23.02637480153789795 ) ) ;
#3871 = CARTESIAN_POINT ( 'NONE',  ( 38.46727988002800913, -7.323121355281222655, -4.536819773745172313 ) ) ;
#3872 = CARTESIAN_POINT ( 'NONE',  ( 31.68988926855799448, 0.000000000000000000, 1.626235259850384418 ) ) ;
#3873 = CARTESIAN_POINT ( 'NONE',  ( 1.555617767666469975, 21.18131178815229987, 4.150713132340920097 ) ) ;
#3874 = DIRECTION ( 'NONE',  ( -0.000000000000000000, -1.000000000000000000, 0.000000000000000000 ) ) ;
#3875 = VERTEX_POINT ( 'NONE', #18995 ) ;
#3876 = CARTESIAN_POINT ( 'NONE',  ( 3.341345536767371005, 19.49937761787746382, 7.593489763050116359 ) ) ;
#3877 = FACE_OUTER_BOUND ( 'NONE', #7700, .T. ) ;
#3878 = LINE ( 'NONE', #15727, #410 ) ;
#3879 = DIRECTION ( 'NONE',  ( 0.2490110332224850509, 0.000000000000000000, -0.9685006480810792739 ) ) ;
#3880 = EDGE_LOOP ( 'NONE', ( #9597, #11365, #14261, #1942 ) ) ;
#3881 = VERTEX_POINT ( 'NONE', #7293 ) ;
#3882 = CARTESIAN_POINT ( 'NONE',  ( 10.85322530146255282, 18.36121671486396778, -3.976481845014243177 ) ) ;
#3883 = DIRECTION ( 'NONE',  ( 0.000000000000000000, 1.000000000000000000, 0.000000000000000000 ) ) ;
#3884 = CARTESIAN_POINT ( 'NONE',  ( 11.87485077258540933, 10.52519879175988038, 0.2400876501387014805 ) ) ;
#3885 = ORIENTED_EDGE ( 'NONE', *, *, #14904, .T. ) ;
#3886 = ORIENTED_EDGE ( 'NONE', *, *, #15205, .F. ) ;
#3887 = FACE_OUTER_BOUND ( 'NONE', #18893, .T. ) ;
#3888 = CARTESIAN_POINT ( 'NONE',  ( 9.462450425703316625, 14.07471438502956218, 7.526408680303447341 ) ) ;
#3889 = CARTESIAN_POINT ( 'NONE',  ( 3.215393543773535256, 17.96135795615357011, 8.214310353060460201 ) ) ;
#3890 = FACE_OUTER_BOUND ( 'NONE', #4134, .T. ) ;
#3891 = AXIS2_PLACEMENT_3D ( 'NONE', #3142, #16748, #1263 ) ;
#3892 = CARTESIAN_POINT ( 'NONE',  ( 5.640316583454905164, 13.99766401133218174, -0.7584365737669227503 ) ) ;
#3893 = LINE ( 'NONE', #15517, #1878 ) ;
#3894 = EDGE_CURVE ( 'NONE', #17254, #18451, #871, .T. ) ;
#3895 = CARTESIAN_POINT ( 'NONE',  ( 11.69298665771319357, 13.72201164258680173, 6.917504522580232518 ) ) ;
#3896 = CARTESIAN_POINT ( 'NONE',  ( 4.780383433206969457, 11.98883979544040201, 4.693647510922787980 ) ) ;
#3897 = CARTESIAN_POINT ( 'NONE',  ( 2.062732473717475035, 11.83352507831272149, 1.765483589054170244 ) ) ;
#3898 = CARTESIAN_POINT ( 'NONE',  ( 0.1227838744961313316, 20.95892070510404182, 5.974958143557400625 ) ) ;
#3899 = DIRECTION ( 'NONE',  ( -0.9987059298363656357, 0.000000000000000000, -0.05085730733808393328 ) ) ;
#3900 = CIRCLE ( 'NONE', #18402, 0.7950200000000005041 ) ;
#3901 = CARTESIAN_POINT ( 'NONE',  ( 3.918141522112466024, 12.81903963674880131, 0.8919207467421174096 ) ) ;
#3902 = CARTESIAN_POINT ( 'NONE',  ( 39.27728671717661513, 0.000000000000000000, -23.95520057284206672 ) ) ;
#3903 = CARTESIAN_POINT ( 'NONE',  ( 66.03921914090641110, -42.42568807200000691, -11.33033647675950029 ) ) ;
#3904 = CARTESIAN_POINT ( 'NONE',  ( 20.94764122044779597, -2.744589957913053269, -13.89552819659893146 ) ) ;
#3905 = AXIS2_PLACEMENT_3D ( 'NONE', #164, #14011, #5237 ) ;
#3906 = CARTESIAN_POINT ( 'NONE',  ( 9.058884679750676128, 128.5105379999999968, -16.32319115207028659 ) ) ;
#3907 = CARTESIAN_POINT ( 'NONE',  ( 11.32837441058685535, 13.16913511479088683, 6.657235606396362471 ) ) ;
#3908 = VERTEX_POINT ( 'NONE', #5745 ) ;
#3909 = LINE ( 'NONE', #17613, #13850 ) ;
#3910 = CARTESIAN_POINT ( 'NONE',  ( 11.15056158858318902, 14.80538177552531742, -3.352690886573022055 ) ) ;
#3911 = CIRCLE ( 'NONE', #18380, 3.175000000000001155 ) ;
#3912 = DIRECTION ( 'NONE',  ( 0.000000000000000000, -1.000000000000000000, 0.000000000000000000 ) ) ;
#3913 = CARTESIAN_POINT ( 'NONE',  ( 0.9804779173902414824, 12.40032227216336125, 6.306356520460885129 ) ) ;
#3914 = ORIENTED_EDGE ( 'NONE', *, *, #2240, .T. ) ;
#3915 = LINE ( 'NONE', #3695, #14894 ) ;
#3916 = AXIS2_PLACEMENT_3D ( 'NONE', #4930, #11677, #8355 ) ;
#3917 = DIRECTION ( 'NONE',  ( -0.2490110332224855227, 0.000000000000000000, 0.9685006480810791629 ) ) ;
#3918 = CIRCLE ( 'NONE', #6733, 0.5080000000000034488 ) ;
#3919 = EDGE_CURVE ( 'NONE', #20253, #7504, #18523, .T. ) ;
#3920 = ORIENTED_EDGE ( 'NONE', *, *, #389, .T. ) ;
#3921 = CARTESIAN_POINT ( 'NONE',  ( 10.20950810520924179, 20.26079639706886226, -1.226483415077589401 ) ) ;
#3922 = CARTESIAN_POINT ( 'NONE',  ( 4.147649111953238155, 20.32216908442184078, 5.402681071153457637 ) ) ;
#3923 = CIRCLE ( 'NONE', #7106, 0.7950200000000005041 ) ;
#3924 = CYLINDRICAL_SURFACE ( 'NONE', #6838, 0.3962400000000008138 ) ;
#3925 = CARTESIAN_POINT ( 'NONE',  ( 5.895566845034227121, 14.03105527214651715, 7.837517794756466039 ) ) ;
#3926 = CARTESIAN_POINT ( 'NONE',  ( 56.91751438644678984, 34.52875999999999834, -20.96198986413465448 ) ) ;
#3927 = VECTOR ( 'NONE', #9899, 1000.000000000000000 ) ;
#3928 = CARTESIAN_POINT ( 'NONE',  ( 20.23468942577036600, -1.359616646866762757, -14.75420580893919542 ) ) ;
#3929 = UNCERTAINTY_MEASURE_WITH_UNIT (LENGTH_MEASURE( 1.000000000000000082E-05 ), #5164, 'distance_accuracy_value', 'NONE');
#3930 = PLANE ( 'NONE',  #12010 ) ;
#3931 = ORIENTED_EDGE ( 'NONE', *, *, #9789, .F. ) ;
#3932 = CARTESIAN_POINT ( 'NONE',  ( 11.33996423452750335, 22.16594858500680232, 2.023480447774197444 ) ) ;
#3933 = LINE ( 'NONE', #19058, #6323 ) ;
#3934 = ORIENTED_EDGE ( 'NONE', *, *, #4790, .F. ) ;
#3935 = CARTESIAN_POINT ( 'NONE',  ( 9.319472022997786098, 16.19024704327322084, -2.854579263552438295 ) ) ;
#3936 = CARTESIAN_POINT ( 'NONE',  ( 13.36143179939526071, 19.43957250000000059, -3.203440815378094886 ) ) ;
#3937 = CARTESIAN_POINT ( 'NONE',  ( 36.51250000000000284, 0.000000000000000000, -10.31875000000000142 ) ) ;
#3939 = CARTESIAN_POINT ( 'NONE',  ( 50.52547294529469468, 38.88803500000000213, -18.64987929725020521 ) ) ;
#3938 = CARTESIAN_POINT ( 'NONE',  ( 3.622151847267213398, 20.92444076583792167, 5.284828060340222677 ) ) ;
#3940 = EDGE_LOOP ( 'NONE', ( #17314, #10341, #7048, #8880, #865, #13918, #11787 ) ) ;
#3941 = VECTOR ( 'NONE', #20801, 1000.000000000000227 ) ;
#3942 = DIRECTION ( 'NONE',  ( -0.000000000000000000, -1.000000000000000000, 0.000000000000000000 ) ) ;
#3943 = VECTOR ( 'NONE', #19960, 1000.000000000000000 ) ;
#3944 = VERTEX_POINT ( 'NONE', #19222 ) ;
#3945 = DIRECTION ( 'NONE',  ( -0.08420877549337300871, 0.000000000000000000, -0.9964481331860212121 ) ) ;
#3946 = EDGE_CURVE ( 'NONE', #18904, #18859, #10609, .T. ) ;
#3947 = CIRCLE ( 'NONE', #1471, 30.16249999999998721 ) ;
#3948 = CARTESIAN_POINT ( 'NONE',  ( 20.08284348270143838, -2.741504599332891257, -14.26371703632316468 ) ) ;
#3949 = ORIENTED_EDGE ( 'NONE', *, *, #4679, .F. ) ;
#3950 = CARTESIAN_POINT ( 'NONE',  ( 12.91596452321051558, 19.43893749999999798, 2.799331278665067479 ) ) ;
#3951 = DIRECTION ( 'NONE',  ( 0.9579671649362032637, 0.000000000000000000, -0.2868778675745010664 ) ) ;
#3952 = DIRECTION ( 'NONE',  ( 0.000000000000000000, 1.000000000000000000, 0.000000000000000000 ) ) ;
#3953 = CIRCLE ( 'NONE', #11369, 0.7950199999999985057 ) ;
#3954 = VECTOR ( 'NONE', #15173, 1000.000000000000114 ) ;
#3955 = ORIENTED_EDGE ( 'NONE', *, *, #2791, .F. ) ;
#3956 = CARTESIAN_POINT ( 'NONE',  ( 59.90456643211351917, 2.586003464000000029, -2.926035437812116946 ) ) ;
#3957 = CARTESIAN_POINT ( 'NONE',  ( 30.50878709810603340, 29.95901653600000003, -19.83971405306587954 ) ) ;
#3958 = DIRECTION ( 'NONE',  ( -0.000000000000000000, -1.000000000000000000, 0.000000000000000000 ) ) ;
#3959 = ORIENTED_EDGE ( 'NONE', *, *, #12542, .T. ) ;
#3960 = ORIENTED_EDGE ( 'NONE', *, *, #4201, .F. ) ;
#3961 = CIRCLE ( 'NONE', #16331, 6.349999999999999645 ) ;
#3962 = B_SPLINE_CURVE_WITH_KNOTS ( 'NONE', 3,
 ( #17142, #5408, #1984, #12173, #10169, #18670, #3767, #11732, #10504, #16913, #7715, #13621, #17249, #18467, #3335, #1653, #8394, #15285 ),
 .UNSPECIFIED., .F., .F.,
 ( 4, 2, 2, 2, 2, 2, 2, 2, 4 ),
 ( 0.003754349818373628987, 0.004223755935673022613, 0.004693162052972417106, 0.005162568170271811599, 0.005631974287571205225, 0.006101380404870598850, 0.006570786522169993343, 0.007040192639469387836, 0.007509598756768781462 ),
 .UNSPECIFIED. ) ;
#3964 = DIRECTION ( 'NONE',  ( 0.000000000000000000, -1.000000000000000000, -0.000000000000000000 ) ) ;
#3963 = CARTESIAN_POINT ( 'NONE',  ( 3.627712153688075869, 17.35305612800781816, -1.455835595266307125 ) ) ;
#3965 = ORIENTED_EDGE ( 'NONE', *, *, #14127, .F. ) ;
#3967 = CARTESIAN_POINT ( 'NONE',  ( 20.13189412415908564, -6.543715966850456311, -14.70988029850133927 ) ) ;
#3966 = CARTESIAN_POINT ( 'NONE',  ( 4.917538461146517825, 11.31976844172629271, 5.235219669757365857 ) ) ;
#3968 = ADVANCED_FACE ( 'NONE', ( #12386 ), #12270, .T. ) ;
#3969 = VERTEX_POINT ( 'NONE', #3872 ) ;
#3970 = ORIENTED_EDGE ( 'NONE', *, *, #12995, .F. ) ;
#3971 = AXIS2_PLACEMENT_3D ( 'NONE', #19107, #7394, #14165 ) ;
#3972 = AXIS2_PLACEMENT_3D ( 'NONE', #82, #12026, #20516 ) ;
#3973 = EDGE_CURVE ( 'NONE', #13907, #8439, #440, .T. ) ;
#3974 = VERTEX_POINT ( 'NONE', #10724 ) ;
#3975 = EDGE_CURVE ( 'NONE', #2248, #2705, #1232, .T. ) ;
#3976 = VECTOR ( 'NONE', #15344, 1000.000000000000000 ) ;
#3977 = CIRCLE ( 'NONE', #16346, 0.5080000000000012284 ) ;
#3978 = CARTESIAN_POINT ( 'NONE',  ( 59.89111109153450485, 34.52875999999999834, -22.14529389979288965 ) ) ;
#3979 = CARTESIAN_POINT ( 'NONE',  ( -16.73439918454169018, 37.15413452960619622, -25.92417111164088084 ) ) ;
#3980 = LINE ( 'NONE', #3760, #7221 ) ;
#3981 = DIRECTION ( 'NONE',  ( 0.2490110332224846623, 0.000000000000000000, -0.9685006480810793850 ) ) ;
#3982 = CARTESIAN_POINT ( 'NONE',  ( 3.426798112698273613, 17.95067475860813744, 8.948262651118973565 ) ) ;
#3983 = EDGE_LOOP ( 'NONE', ( #8656, #3299, #10213, #20181 ) ) ;
#3984 = CARTESIAN_POINT ( 'NONE',  ( 1.165675658960684258, 19.99706093811970220, 1.906448648540375324 ) ) ;
#3985 = CARTESIAN_POINT ( 'NONE',  ( 9.335363283976800375, 34.52875999999999834, -14.20581391854862474 ) ) ;
#3986 = LINE ( 'NONE', #5518, #8848 ) ;
#3987 = FACE_OUTER_BOUND ( 'NONE', #5274, .T. ) ;
#3988 = VECTOR ( 'NONE', #11861, 1000.000000000000000 ) ;
#3989 = ORIENTED_EDGE ( 'NONE', *, *, #15440, .F. ) ;
#3990 = ORIENTED_EDGE ( 'NONE', *, *, #12213, .F. ) ;
#3991 = CARTESIAN_POINT ( 'NONE',  ( 11.85589261522914128, 21.52809012965692403, -1.417360321702582970 ) ) ;
#3992 = CARTESIAN_POINT ( 'NONE',  ( 29.37324403177899868, 30.56064500000000095, -10.70578951775076071 ) ) ;
#3993 = CARTESIAN_POINT ( 'NONE',  ( 11.32652070754218698, 11.63326539784401170, -2.087448442563799134 ) ) ;
#3994 = ORIENTED_EDGE ( 'NONE', *, *, #4822, .F. ) ;
#3995 = EDGE_CURVE ( 'NONE', #4404, #11521, #17573, .T. ) ;
#3996 = ORIENTED_EDGE ( 'NONE', *, *, #19377, .F. ) ;
#3997 = DIRECTION ( 'NONE',  ( 0.000000000000000000, -1.000000000000000000, 0.000000000000000000 ) ) ;
#3998 = CARTESIAN_POINT ( 'NONE',  ( 7.482895972121536232, 12.31879885248479667, -1.218862190161812409 ) ) ;
#3999 = AXIS2_PLACEMENT_3D ( 'NONE', #9753, #16516, #17162 ) ;
#4000 = CARTESIAN_POINT ( 'NONE',  ( 2.943417611999118666, 20.19995037221810108, 2.177142770243966741 ) ) ;
#4001 = DIRECTION ( 'NONE',  ( -0.2490110332224850231, 0.000000000000000000, 0.9685006480810791629 ) ) ;
#4002 = CARTESIAN_POINT ( 'NONE',  ( 5.677412915715525976, 13.63288455579914071, -0.5314653111491820514 ) ) ;
#4003 = ADVANCED_FACE ( 'NONE', ( #2085 ), #2644, .T. ) ;
#4004 = DIRECTION ( 'NONE',  ( 0.7421532822901572013, 0.000000000000000000, -0.6702301885068637777 ) ) ;
#4005 = AXIS2_PLACEMENT_3D ( 'NONE', #4522, #11259, #7725 ) ;
#4006 = CYLINDRICAL_SURFACE ( 'NONE', #16938, 1.587499999999998579 ) ;
#4007 = CARTESIAN_POINT ( 'NONE',  ( 9.728942020902382026, 11.81448552380872208, -1.613679459648534653 ) ) ;
#4008 = CARTESIAN_POINT ( 'NONE',  ( -0.3522849415351315683, 21.11360319320700185, 4.780382278449337718 ) ) ;
#4009 = CARTESIAN_POINT ( 'NONE',  ( 0.2729244852844739944, 20.85630707936518036, 6.375157578189681651 ) ) ;
#4010 = VECTOR ( 'NONE', #8521, 1000.000000000000000 ) ;
#4011 = DIRECTION ( 'NONE',  ( 0.7421532822901579785, 0.000000000000000000, -0.6702301885068628895 ) ) ;
#4012 = CARTESIAN_POINT ( 'NONE',  ( 0.7458913913427336340, 12.12637795047220202, 4.864350555078584826 ) ) ;
#4013 = PLANE ( 'NONE',  #20830 ) ;
#4014 = DIRECTION ( 'NONE',  ( 0.7421532822901569793, 0.000000000000000000, -0.6702301885068642218 ) ) ;
#4015 = CARTESIAN_POINT ( 'NONE',  ( 14.63395006230149775, 2.144152496841746469, -15.86064623020511100 ) ) ;
#4016 = DIRECTION ( 'NONE',  ( -0.07875956036501312318, 0.000000000000000000, 0.9968936410927243807 ) ) ;
#4017 = CARTESIAN_POINT ( 'NONE',  ( 9.925807051316079210, 10.75363849649213144, 0.5961705298080919313 ) ) ;
#4018 = EDGE_LOOP ( 'NONE', ( #3147, #1747 ) ) ;
#4019 = ADVANCED_FACE ( 'NONE', ( #15719 ), #19433, .F. ) ;
#4020 = AXIS2_PLACEMENT_3D ( 'NONE', #11023, #13136, #9684 ) ;
#4021 = DIRECTION ( 'NONE',  ( 0.000000000000000000, 1.000000000000000000, 0.000000000000000000 ) ) ;
#4022 = EDGE_CURVE ( 'NONE', #5923, #6054, #5451, .T. ) ;
#4023 = CARTESIAN_POINT ( 'NONE',  ( 12.07662037374150188, 11.20872780036083149, 1.062083825547142091 ) ) ;
#4024 = CARTESIAN_POINT ( 'NONE',  ( 5.369103247086697728, 15.71570224551708428, -2.120753809282792002 ) ) ;
#4025 = DIRECTION ( 'NONE',  ( 0.000000000000000000, 1.000000000000000000, 0.000000000000000000 ) ) ;
#4026 = CARTESIAN_POINT ( 'NONE',  ( 2.745045924436487983, 19.21529397045534182, 7.464326575930528840 ) ) ;
#4027 = ORIENTED_EDGE ( 'NONE', *, *, #15919, .T. ) ;
#4028 = ITEM_DEFINED_TRANSFORMATION ( 'NONE', 'NONE', #2773,  #2234 ) ;
#4029 = LINE ( 'NONE', #19376, #8618 ) ;
#4030 = AXIS2_PLACEMENT_3D ( 'NONE', #14713, #8908, #2279 ) ;
#4031 = VERTEX_POINT ( 'NONE', #16044 ) ;
#4032 = CARTESIAN_POINT ( 'NONE',  ( 9.207133947949060371, 21.14801334772412034, 1.738871791010894174 ) ) ;
#4033 = VECTOR ( 'NONE', #2083, 1000.000000000000114 ) ;
#4034 = CARTESIAN_POINT ( 'NONE',  ( 11.95356391707709243, 20.94917700551698303, 3.645593293397387136 ) ) ;
#4035 = CARTESIAN_POINT ( 'NONE',  ( 30.47347900023190803, 0.000000000000000000, -8.148724574017967015 ) ) ;
#4036 = CARTESIAN_POINT ( 'NONE',  ( 16.45009588711971560, 1.051937461999462364, -15.31736409357231388 ) ) ;
#4037 = CYLINDRICAL_SURFACE ( 'NONE', #17325, 1.983739999999999393 ) ;
#4038 = VERTEX_POINT ( 'NONE', #7618 ) ;
#4039 = CARTESIAN_POINT ( 'NONE',  ( 11.22049204336262029, 14.97478453086299766, 6.637898145237717706 ) ) ;
#4040 = CARTESIAN_POINT ( 'NONE',  ( 9.107295249990597696, 21.95697059135326512, 1.669600826508311320 ) ) ;
#4041 = VECTOR ( 'NONE', #21286, 1000.000000000000000 ) ;
#4042 = FACE_OUTER_BOUND ( 'NONE', #1426, .T. ) ;
#4043 = VERTEX_POINT ( 'NONE', #13953 ) ;
#4044 = EDGE_CURVE ( 'NONE', #20031, #14428, #17466, .T. ) ;
#4045 = CARTESIAN_POINT ( 'NONE',  ( 9.431633194775894680, 13.20025053816172189, -1.758368973243622957 ) ) ;
#4046 = CARTESIAN_POINT ( 'NONE',  ( 12.88040283537677588, 20.23395749999999893, -0.09070320285213756550 ) ) ;
#4047 = CARTESIAN_POINT ( 'NONE',  ( 66.79943102505561114, 36.51313500000000545, -12.07331878313145168 ) ) ;
#4049 = CARTESIAN_POINT ( 'NONE',  ( 43.49132289107146931, 0.000000000000000000, 4.686923926377883021 ) ) ;
#4048 = CARTESIAN_POINT ( 'NONE',  ( 5.088084651243378609, 15.68947463651248420, 8.601854303313373862 ) ) ;
#4050 = ORIENTED_EDGE ( 'NONE', *, *, #14324, .T. ) ;
#4051 = CARTESIAN_POINT ( 'NONE',  ( 7.156657753775511388, 11.88141511607538092, 6.132460277425193063 ) ) ;
#4052 = CIRCLE ( 'NONE', #16417, 0.7950199999999997269 ) ;
#4053 = CARTESIAN_POINT ( 'NONE',  ( 2.520748753591570690, 5.548947500000001476, -24.56335908395234924 ) ) ;
#4054 = CARTESIAN_POINT ( 'NONE',  ( 39.82201269448036385, -6.200394330680151889, -3.101178208336223818 ) ) ;
#4055 = ORIENTED_EDGE ( 'NONE', *, *, #20746, .F. ) ;
#4056 = CARTESIAN_POINT ( 'NONE',  ( 19.35734219002929635, 0.4354800424330582675, -15.01894665276165242 ) ) ;
#4057 = CARTESIAN_POINT ( 'NONE',  ( 0.03417565917660739944, 14.83535024179863804, 1.090746620095099040 ) ) ;
#4058 = CARTESIAN_POINT ( 'NONE',  ( 19.41542498887948653, -5.356659253819461952, -14.11969569052875606 ) ) ;
#4059 = ORIENTED_EDGE ( 'NONE', *, *, #12490, .T. ) ;
#4060 = DIRECTION ( 'NONE',  ( 0.9129422336036127072, 0.000000000000000000, -0.4080888115384278536 ) ) ;
#4061 = CARTESIAN_POINT ( 'NONE',  ( 2.146289851715664998, 18.00879166459082370, 0.3733188029809513253 ) ) ;
#4062 = CARTESIAN_POINT ( 'NONE',  ( 13.02203208521239652, 11.26511959538250096, 4.614517720664577105 ) ) ;
#4063 = LINE ( 'NONE', #10805, #6788 ) ;
#4064 = AXIS2_PLACEMENT_3D ( 'NONE', #2535, #2202, #8943 ) ;
#4065 = FACE_OUTER_BOUND ( 'NONE', #18135, .T. ) ;
#4066 = ORIENTED_EDGE ( 'NONE', *, *, #2487, .T. ) ;
#4067 = DIRECTION ( 'NONE',  ( -0.2868778675745010664, 0.000000000000000000, -0.9579671649362032637 ) ) ;
#4069 = DIRECTION ( 'NONE',  ( 0.000000000000000000, -1.000000000000000000, 0.000000000000000000 ) ) ;
#4068 = DIRECTION ( 'NONE',  ( 0.3928209820863007851, 0.000000000000000000, -0.9196149607486571176 ) ) ;
#4070 = EDGE_LOOP ( 'NONE', ( #8707, #20950, #17413, #12279 ) ) ;
#4071 = ORIENTED_EDGE ( 'NONE', *, *, #19305, .F. ) ;
#4072 = EDGE_CURVE ( 'NONE', #8133, #17060, #11118, .T. ) ;
#4074 = CARTESIAN_POINT ( 'NONE',  ( 46.03750000000000142, -9.531985000000000596, -10.31874999999999964 ) ) ;
#4073 = CARTESIAN_POINT ( 'NONE',  ( 3.279053066004760542, 11.89954130989696246, 6.881081710522694905 ) ) ;
#4075 = ORIENTED_EDGE ( 'NONE', *, *, #14515, .F. ) ;
#4076 = CARTESIAN_POINT ( 'NONE',  ( 5.570283759808590140, 14.18670928006132215, 8.353561429919604819 ) ) ;
#4077 = VERTEX_POINT ( 'NONE', #17901 ) ;
#4078 = VERTEX_POINT ( 'NONE', #21314 ) ;
#4079 = CIRCLE ( 'NONE', #4436, 5.158740000000001658 ) ;
#4080 = ORIENTED_EDGE ( 'NONE', *, *, #13166, .F. ) ;
#4081 = EDGE_CURVE ( 'NONE', #15859, #10888, #8991, .T. ) ;
#4082 = DIRECTION ( 'NONE',  ( 0.000000000000000000, 0.000000000000000000, 1.000000000000000000 ) ) ;
#4083 = LINE ( 'NONE', #3979, #8596 ) ;
#4084 = DIRECTION ( 'NONE',  ( 0.000000000000000000, 1.000000000000000000, 0.000000000000000000 ) ) ;
#4085 = CARTESIAN_POINT ( 'NONE',  ( 3.010873720258615549, 19.62469427726395921, 7.998214828720064951 ) ) ;
#4086 = ORIENTED_EDGE ( 'NONE', *, *, #13438, .T. ) ;
#4087 = CARTESIAN_POINT ( 'NONE',  ( 1.189115539264649524, 19.87555530259703929, 7.508218902050214361 ) ) ;
#4088 = LINE ( 'NONE', #2316, #16669 ) ;
#4089 = CARTESIAN_POINT ( 'NONE',  ( 27.87822510359947614, 0.000000000000000000, -8.893823290944665061 ) ) ;
#4090 = CARTESIAN_POINT ( 'NONE',  ( 28.38195592936287781, 40.07707250000000698, -13.81504834214261024 ) ) ;
#4091 = AXIS2_PLACEMENT_3D ( 'NONE', #12998, #3131, #6561 ) ;
#4092 = CARTESIAN_POINT ( 'NONE',  ( -2.845411283647486300, 33.32892749999999893, -5.196881601526627925 ) ) ;
#4093 = ORIENTED_EDGE ( 'NONE', *, *, #17551, .T. ) ;
#4094 = ORIENTED_EDGE ( 'NONE', *, *, #20018, .T. ) ;
#4095 = EDGE_CURVE ( 'NONE', #19126, #9142, #6879, .T. ) ;
#4096 = CARTESIAN_POINT ( 'NONE',  ( 8.681707164006697397, 21.55462128078298178, 1.846373227260097227 ) ) ;
#4097 = EDGE_CURVE ( 'NONE', #13820, #966, #9700, .T. ) ;
#4099 = DIRECTION ( 'NONE',  ( 0.000000000000000000, 1.000000000000000000, -0.000000000000000000 ) ) ;
#4098 = CARTESIAN_POINT ( 'NONE',  ( 30.50878709810603340, -1.983739999999999837, -19.83971405306587954 ) ) ;
#4100 = CARTESIAN_POINT ( 'NONE',  ( 12.36232094770518408, 10.46176486781214088, 2.258949820783138218 ) ) ;
#4101 = ORIENTED_EDGE ( 'NONE', *, *, #6921, .T. ) ;
#4102 = ORIENTED_EDGE ( 'NONE', *, *, #5574, .T. ) ;
#4103 = DIRECTION ( 'NONE',  ( 0.5734623443633278805, 0.8192319205190407017, 0.000000000000000000 ) ) ;
#4104 = CARTESIAN_POINT ( 'NONE',  ( 7.762073279291525019, 19.65299917282199971, -1.873378395566488219 ) ) ;
#4105 = CARTESIAN_POINT ( 'NONE',  ( 4.950627004242664775, 12.10224027996176233, 5.328968407580981115 ) ) ;
#4106 = PLANE ( 'NONE',  #6987 ) ;
#4107 = CARTESIAN_POINT ( 'NONE',  ( 5.587073591125067296, 15.32039277778152275, -1.277284589391624481 ) ) ;
#4108 = CARTESIAN_POINT ( 'NONE',  ( 38.97454265763864356, 37.69740999999999786, -3.928105264594607071 ) ) ;
#4109 = DIRECTION ( 'NONE',  ( -0.9685006480810794960, 0.000000000000000000, -0.2490110332224836354 ) ) ;
#4110 = CARTESIAN_POINT ( 'NONE',  ( 4.592488401674089005, 11.87781438748830531, 3.847380809352867193 ) ) ;
#4111 = EDGE_CURVE ( 'NONE', #97, #14616, #14714, .T. ) ;
#4112 = CARTESIAN_POINT ( 'NONE',  ( 6.831402082338472681, 20.09449018309318191, 7.036973853986666860 ) ) ;
#4113 = CARTESIAN_POINT ( 'NONE',  ( 8.011380105705496746, 6.343967500000000648, -19.05252355006962617 ) ) ;
#4114 = FACE_OUTER_BOUND ( 'NONE', #4512, .T. ) ;
#4115 = CARTESIAN_POINT ( 'NONE',  ( 3.170692993479493182, 17.96108129601270775, 8.227029222725301238 ) ) ;
#4116 = CARTESIAN_POINT ( 'NONE',  ( 12.62386444219163373, 13.08957250000000094, -17.86660850434754266 ) ) ;
#4117 = DIRECTION ( 'NONE',  ( 0.000000000000000000, 0.000000000000000000, -1.000000000000000000 ) ) ;
#4118 = CARTESIAN_POINT ( 'NONE',  ( 12.35899892427300983, 0.8773483136192000709, -16.54479250898838671 ) ) ;
#4119 = ORIENTED_EDGE ( 'NONE', *, *, #8322, .F. ) ;
#4120 = CARTESIAN_POINT ( 'NONE',  ( 66.03921914090641110, 1.984375000000000000, -10.93409647675949969 ) ) ;
#4121 = EDGE_CURVE ( 'NONE', #8727, #20861, #19600, .T. ) ;
#4122 = CARTESIAN_POINT ( 'NONE',  ( 11.36994341220144022, 13.54146173944704579, 6.880576314206986233 ) ) ;
#4123 = ORIENTED_EDGE ( 'NONE', *, *, #10853, .T. ) ;
#4124 = DIRECTION ( 'NONE',  ( 0.9488823340533351081, -0.2002559181062070481, 0.2439669719140998283 ) ) ;
#4125 = CARTESIAN_POINT ( 'NONE',  ( 5.510835403679958056, 13.03497559724449850, -1.051663230879403166 ) ) ;
#4126 = LINE ( 'NONE', #12647, #14824 ) ;
#4127 = ORIENTED_EDGE ( 'NONE', *, *, #21754, .T. ) ;
#4128 =( NAMED_UNIT ( * ) SI_UNIT ( $, .STERADIAN. ) SOLID_ANGLE_UNIT ( ) );
#4129 = EDGE_CURVE ( 'NONE', #21761, #21868, #3083, .T. ) ;
#4130 = CARTESIAN_POINT ( 'NONE',  ( 5.545311189636909610, 20.74516219335661660, 3.520903296636215707 ) ) ;
#4131 = CIRCLE ( 'NONE', #12241, 3.175000000000000711 ) ;
#4132 = FACE_BOUND ( 'NONE', #11763, .T. ) ;
#4133 = CARTESIAN_POINT ( 'NONE',  ( 20.10134609765169245, 0.5637867123784654488, -14.37936376174423359 ) ) ;
#4134 = EDGE_LOOP ( 'NONE', ( #20667, #11265, #16524, #15462 ) ) ;
#4135 = CARTESIAN_POINT ( 'NONE',  ( 5.901462123111614666, 12.70293317459338134, 0.1691424549115569387 ) ) ;
#4136 = ADVANCED_FACE ( 'NONE', ( #14606 ), #21647, .T. ) ;
#4137 = CARTESIAN_POINT ( 'NONE',  ( 9.693733691225084215, 18.90712183571880090, -2.322483269049387733 ) ) ;
#4138 = CYLINDRICAL_SURFACE ( 'NONE', #9858, 1.983739999999999837 ) ;
#4139 = ADVANCED_FACE ( 'NONE', ( #6510 ), #13270, .T. ) ;
#4140 = DIRECTION ( 'NONE',  ( 0.000000000000000000, 1.000000000000000000, -0.000000000000000000 ) ) ;
#4141 = EDGE_CURVE ( 'NONE', #16776, #1622, #4079, .T. ) ;
#4142 = DIRECTION ( 'NONE',  ( 0.000000000000000000, 1.000000000000000000, 0.000000000000000000 ) ) ;
#4143 = CARTESIAN_POINT ( 'NONE',  ( 5.450687119353768928, 17.48300910350427628, 8.674115758454949088 ) ) ;
#4144 = UNCERTAINTY_MEASURE_WITH_UNIT (LENGTH_MEASURE( 1.000000000000000082E-05 ), #9340, 'distance_accuracy_value', 'NONE');
#4145 = DIRECTION ( 'NONE',  ( 0.000000000000000000, 1.000000000000000000, 0.000000000000000000 ) ) ;
#4146 = CIRCLE ( 'NONE', #16510, 8.929687500000000000 ) ;
#4147 = ORIENTED_EDGE ( 'NONE', *, *, #11526, .T. ) ;
#4148 = CARTESIAN_POINT ( 'NONE',  ( 9.136086461789291846, 18.56746232396120533, 7.683010205099245482 ) ) ;
#4149 = CARTESIAN_POINT ( 'NONE',  ( 52.65752393886089067, 39.94029975385505082, -17.16880761802969957 ) ) ;
#4150 = ORIENTED_EDGE ( 'NONE', *, *, #21680, .F. ) ;
#4151 = CARTESIAN_POINT ( 'NONE',  ( 9.371701772490553140, 16.88370700927627155, -2.834813229451389027 ) ) ;
#4152 = CARTESIAN_POINT ( 'NONE',  ( 22.02657784715807665, -1.983739999999999393, -12.98906981665815330 ) ) ;
#4153 = CARTESIAN_POINT ( 'NONE',  ( 0.2090372314103253748, 20.09402757005803153, 6.163100425531474080 ) ) ;
#4155 = CARTESIAN_POINT ( 'NONE',  ( -12.20004626880064080, -0.3962399999999990929, -1.006347609994785008 ) ) ;
#4154 = CARTESIAN_POINT ( 'NONE',  ( 4.037559778546858880, 20.21972024448168170, 0.7539604779301642967 ) ) ;
#4156 = EDGE_LOOP ( 'NONE', ( #17793, #20594, #95, #8512 ) ) ;
#4157 = DIRECTION ( 'NONE',  ( 0.000000000000000000, 1.000000000000000000, 0.000000000000000000 ) ) ;
#4158 = CARTESIAN_POINT ( 'NONE',  ( 39.70799623749501706, -5.757505969760286391, -3.200701455436412601 ) ) ;
#4159 = ORIENTED_EDGE ( 'NONE', *, *, #11354, .T. ) ;
#4160 = CARTESIAN_POINT ( 'NONE',  ( 19.34541047516490053, 0.4253635554462941171, -15.02868439565010839 ) ) ;
#4161 = VECTOR ( 'NONE', #7493, 1000.000000000000000 ) ;
#4162 = CARTESIAN_POINT ( 'NONE',  ( 11.73925543172950015, -4.504504147575669748, -15.65183323565414675 ) ) ;
#4163 = VERTEX_POINT ( 'NONE', #14817 ) ;
#4164 = DIRECTION ( 'NONE',  ( -0.9987059298363656357, 0.000000000000000000, -0.05085730733808393328 ) ) ;
#4165 = EDGE_CURVE ( 'NONE', #2030, #13169, #14691, .T. ) ;
#4166 = CARTESIAN_POINT ( 'NONE',  ( 9.235757461302830151, 17.37326356681460382, -3.689043915829297582 ) ) ;
#4167 = DIRECTION ( 'NONE',  ( -0.9964481331860212121, 0.000000000000000000, 0.08420877549337300871 ) ) ;
#4168 = FACE_OUTER_BOUND ( 'NONE', #16376, .T. ) ;
#4169 = ORIENTED_EDGE ( 'NONE', *, *, #2312, .T. ) ;
#4170 = CARTESIAN_POINT ( 'NONE',  ( 49.09065990372640442, 0.000000000000000000, -26.70549589918839928 ) ) ;
#4172 = CARTESIAN_POINT ( 'NONE',  ( 38.28489021960990613, 38.88803500000000213, 2.732679409805250703 ) ) ;
#4171 = DIRECTION ( 'NONE',  ( -0.000000000000000000, -1.000000000000000000, 0.000000000000000000 ) ) ;
#4173 = VERTEX_POINT ( 'NONE', #16470 ) ;
#4174 = ORIENTED_EDGE ( 'NONE', *, *, #19187, .F. ) ;
#4175 = FACE_OUTER_BOUND ( 'NONE', #9255, .T. ) ;
#4177 = LINE ( 'NONE', #15923, #16631 ) ;
#4176 = CARTESIAN_POINT ( 'NONE',  ( 5.003479159263154230, 21.41895532286982018, 1.986973093797242074 ) ) ;
#4178 = ORIENTED_EDGE ( 'NONE', *, *, #18406, .T. ) ;
#4179 = CARTESIAN_POINT ( 'NONE',  ( 3.620832965735171438, 17.22857179101344016, -1.359620387843638367 ) ) ;
#4180 = VERTEX_POINT ( 'NONE', #1302 ) ;
#4181 = ORIENTED_EDGE ( 'NONE', *, *, #12897, .T. ) ;
#4182 =( GEOMETRIC_REPRESENTATION_CONTEXT ( 3 ) GLOBAL_UNCERTAINTY_ASSIGNED_CONTEXT ( ( #5236 ) ) GLOBAL_UNIT_ASSIGNED_CONTEXT ( ( #6240, #11334, #2715 ) ) REPRESENTATION_CONTEXT ( 'NONE', 'WORKASPACE' ) );
#4183 = CARTESIAN_POINT ( 'NONE',  ( 1.255127740655926250, 12.99292128794711232, 7.191113729468309401 ) ) ;
#4184 = ORIENTED_EDGE ( 'NONE', *, *, #18151, .T. ) ;
#4185 = EDGE_CURVE ( 'NONE', #20863, #16425, #19251, .T. ) ;
#4186 = CIRCLE ( 'NONE', #2056, 0.7950200000000011702 ) ;
#4187 = B_SPLINE_CURVE_WITH_KNOTS ( 'NONE', 3,
 ( #21557, #19462, #9509, #4765 ),
 .UNSPECIFIED., .F., .F.,
 ( 4, 4 ),
 ( 0.008316203670685974950, 0.009146310752383313147 ),
 .UNSPECIFIED. ) ;
#4188 = CARTESIAN_POINT ( 'NONE',  ( -4.728951812473551897, 26.98019749999999917, -29.02782796843600011 ) ) ;
#4189 = CARTESIAN_POINT ( 'NONE',  ( 64.66604708500285881, -1.983739999999999837, -11.54913207920052720 ) ) ;
#4190 = CARTESIAN_POINT ( 'NONE',  ( 1.535814226138735528, 23.46100396823117862, 8.688060833667504923 ) ) ;
#4191 = DIRECTION ( 'NONE',  ( 0.000000000000000000, 1.000000000000000000, 0.000000000000000000 ) ) ;
#4192 = CARTESIAN_POINT ( 'NONE',  ( 2.471328934078918849, 11.32048519468527203, 3.459614447656988112 ) ) ;
#4193 = VERTEX_POINT ( 'NONE', #4420 ) ;
#4194 = CARTESIAN_POINT ( 'NONE',  ( 1.614653659784055284, 18.72099911278871787, 8.534676711928359083 ) ) ;
#4195 = CARTESIAN_POINT ( 'NONE',  ( 31.02798609601340729, 34.52875999999999834, -5.485920235548950252 ) ) ;
#4196 = CARTESIAN_POINT ( 'NONE',  ( 13.20954647625931777, 22.11403031342653591, 1.997722137595396852 ) ) ;
#4197 = CARTESIAN_POINT ( 'NONE',  ( 3.805353748838121053, 34.52875999999999834, -22.18284873352824960 ) ) ;
#4198 = VECTOR ( 'NONE', #7115, 1000.000000000000000 ) ;
#4199 = ORIENTED_EDGE ( 'NONE', *, *, #3301, .F. ) ;
#4200 = ORIENTED_EDGE ( 'NONE', *, *, #14543, .F. ) ;
#4201 = EDGE_CURVE ( 'NONE', #17126, #19423, #15035, .T. ) ;
#4202 = CARTESIAN_POINT ( 'NONE',  ( 12.44599801692499241, 11.60770318476056140, 4.553026975270451970 ) ) ;
#4204 = PLANE ( 'NONE',  #7124 ) ;
#4203 = DIRECTION ( 'NONE',  ( -0.000000000000000000, -1.000000000000000000, 0.000000000000000000 ) ) ;
#4205 = CARTESIAN_POINT ( 'NONE',  ( 12.07372255579661946, 10.41170888677670270, 1.064424525701137103 ) ) ;
#4206 = ORIENTED_EDGE ( 'NONE', *, *, #8093, .F. ) ;
#4207 = ORIENTED_EDGE ( 'NONE', *, *, #10301, .T. ) ;
#4208 = CARTESIAN_POINT ( 'NONE',  ( 29.45491884992628329, 36.51313500000000545, -15.58809351040512325 ) ) ;
#4209 = VECTOR ( 'NONE', #18646, 1000.000000000000000 ) ;
#4210 = CARTESIAN_POINT ( 'NONE',  ( 7.389527843533306495, 12.82742614983489737, -1.666067054070730302 ) ) ;
#4211 = CARTESIAN_POINT ( 'NONE',  ( 17.34610635302146164, 19.43957250000000059, -18.70138818597152053 ) ) ;
#4212 = CARTESIAN_POINT ( 'NONE',  ( -0.06046748314524758028, -7.547927499999999235, -21.12787488008327585 ) ) ;
#4213 = CARTESIAN_POINT ( 'NONE',  ( 6.633674063341000071, 20.34825906491803238, 0.8060356396175938354 ) ) ;
#4214 = CARTESIAN_POINT ( 'NONE',  ( 7.322682645118421263, 14.91079802554269307, 7.412562723462624348 ) ) ;
#4215 = DIRECTION ( 'NONE',  ( 0.08420877549337300871, 0.000000000000000000, 0.9964481331860212121 ) ) ;
#4216 = AXIS2_PLACEMENT_3D ( 'NONE', #14320, #20804, #1019 ) ;
#4217 = EDGE_CURVE ( 'NONE', #14117, #20833, #5464, .T. ) ;
#4218 = CARTESIAN_POINT ( 'NONE',  ( 13.21515623208546764, 11.34183091107056107, 4.504288056618959146 ) ) ;
#4219 = EDGE_CURVE ( 'NONE', #14428, #3833, #3712, .T. ) ;
#4220 = PLANE ( 'NONE',  #701 ) ;
#4221 = CARTESIAN_POINT ( 'NONE',  ( 5.559603178726561623, 13.84461567157916662, 8.313571739785118098 ) ) ;
#4222 = CARTESIAN_POINT ( 'NONE',  ( -0.1072886869958045164, 21.03162608686091062, 5.359064832216835939 ) ) ;
#4223 = AXIS2_PLACEMENT_3D ( 'NONE', #19177, #7464, #16104 ) ;
#4224 = CARTESIAN_POINT ( 'NONE',  ( 39.00487391864218267, 37.69864044684034354, -3.894748490052650780 ) ) ;
#4225 = CARTESIAN_POINT ( 'NONE',  ( 6.982204062069592432, 12.34291428558256065, 5.600203218024798701 ) ) ;
#4226 = DIRECTION ( 'NONE',  ( -0.7532174416907914116, 0.000000000000000000, -0.6577716059034314222 ) ) ;
#4227 = CARTESIAN_POINT ( 'NONE',  ( 65.64431122251959039, 32.54502000000000095, -11.29787305743958115 ) ) ;
#4228 = CARTESIAN_POINT ( 'NONE',  ( 20.94643432978362441, -2.720492664379854819, -13.89672058998338855 ) ) ;
#4229 = EDGE_LOOP ( 'NONE', ( #17611, #14707, #2097, #5148 ) ) ;
#4230 = CARTESIAN_POINT ( 'NONE',  ( 61.04701390398659555, 0.000000000000000000, -15.15157976445104993 ) ) ;
#4231 = VECTOR ( 'NONE', #14776, 1000.000000000000000 ) ;
#4232 = CARTESIAN_POINT ( 'NONE',  ( 11.18085364544609384, 12.25195592965612690, 5.936477548793301473 ) ) ;
#4233 = ORIENTED_EDGE ( 'NONE', *, *, #17908, .F. ) ;
#4234 = VECTOR ( 'NONE', #12383, 1000.000000000000000 ) ;
#4235 = CARTESIAN_POINT ( 'NONE',  ( 25.99163424860619642, 1.095943520706746055, 10.50611347932359863 ) ) ;
#4236 = CARTESIAN_POINT ( 'NONE',  ( 5.445077015079114346, 13.57693074510927289, -1.403816391461112589 ) ) ;
#4237 = DIRECTION ( 'NONE',  ( 0.2490110332224850231, 0.000000000000000000, -0.9685006480810791629 ) ) ;
#4238 = ORIENTED_EDGE ( 'NONE', *, *, #18010, .F. ) ;
#4239 = EDGE_CURVE ( 'NONE', #1356, #11142, #17495, .T. ) ;
#4240 = CARTESIAN_POINT ( 'NONE',  ( -1.345424459097947834, 20.24316500000000119, 2.648158502653860324 ) ) ;
#4241 = AXIS2_PLACEMENT_3D ( 'NONE', #5333, #20143, #18604 ) ;
#4242 =( BOUNDED_CURVE ( )  B_SPLINE_CURVE ( 3, ( #3581, #17067, #6674, #20146 ),
 .UNSPECIFIED., .F., .F. ) 
 B_SPLINE_CURVE_WITH_KNOTS ( ( 4, 4 ),
 ( 0.000000000000000000, 1.570796326786294994 ),
 .UNSPECIFIED. ) 
 CURVE ( )  GEOMETRIC_REPRESENTATION_ITEM ( )  RATIONAL_B_SPLINE_CURVE ( ( 1.000000000000000000, 0.8047378541263923157, 0.8047378541263923157, 1.000000000000000000 ) ) 
 REPRESENTATION_ITEM ( '' )  );
#4243 = DIRECTION ( 'NONE',  ( 1.000000000000000000, 0.000000000000000000, 0.000000000000000000 ) ) ;
#4244 = ADVANCED_FACE ( 'NONE', ( #18226 ), #21201, .T. ) ;
#4245 = ORIENTED_EDGE ( 'NONE', *, *, #8143, .F. ) ;
#4246 = CARTESIAN_POINT ( 'NONE',  ( 11.22474155257526007, 14.44257473674272241, -3.359826663698572080 ) ) ;
#4247 = ADVANCED_FACE ( 'NONE', ( #13048 ), #74, .F. ) ;
#4248 = AXIS2_PLACEMENT_3D ( 'NONE', #16881, #20186, #406 ) ;
#4249 = VECTOR ( 'NONE', #3598, 1000.000000000000000 ) ;
#4250 = CARTESIAN_POINT ( 'NONE',  ( 10.71187475869725247, 21.11843953786754113, 0.2883095389576884049 ) ) ;
#4251 = DIRECTION ( 'NONE',  ( 0.000000000000000000, 0.000000000000000000, -1.000000000000000000 ) ) ;
#4252 = DIRECTION ( 'NONE',  ( 0.000000000000000000, 1.000000000000000000, 0.000000000000000000 ) ) ;
#4253 = CARTESIAN_POINT ( 'NONE',  ( 39.93069333241964358, 39.05073723955329967, -3.008993689095917023 ) ) ;
#4254 = CARTESIAN_POINT ( 'NONE',  ( 3.288597934804766698, 21.28193718814916480, 3.125135824630198567 ) ) ;
#4255 = CARTESIAN_POINT ( 'NONE',  ( 61.60152099976809126, 32.54502000000000095, -12.48877542598203405 ) ) ;
#4256 = CIRCLE ( 'NONE', #21541, 9.524999999999998579 ) ;
#4257 = EDGE_LOOP ( 'NONE', ( #1025, #7550 ) ) ;
#4258 = CARTESIAN_POINT ( 'NONE',  ( 52.19854938732527216, 38.88803500000000213, -17.58284632693144189 ) ) ;
#4259 = VERTEX_POINT ( 'NONE', #8689 ) ;
#4260 = CARTESIAN_POINT ( 'NONE',  ( 12.40139705607254861, 19.98821005853033483, 4.883289743443808284 ) ) ;
#4261 = DIRECTION ( 'NONE',  ( -0.9964481331860211011, 0.000000000000000000, 0.08420877549337349444 ) ) ;
#4262 = CARTESIAN_POINT ( 'NONE',  ( 1.363855527533811562, 17.01011102508672224, 8.799023506260708061 ) ) ;
#4263 = AXIS2_PLACEMENT_3D ( 'NONE', #11759, #1675, #10089 ) ;
#4265 = DIRECTION ( 'NONE',  ( 0.9943660382494290406, 0.000000000000000000, -0.1060008583745199739 ) ) ;
#4264 = CARTESIAN_POINT ( 'NONE',  ( 1.363973292582373320, 16.43321537790008335, -0.2831975433082900562 ) ) ;
#4266 = VERTEX_POINT ( 'NONE', #13587 ) ;
#4267 =( NAMED_UNIT ( * ) SI_UNIT ( $, .STERADIAN. ) SOLID_ANGLE_UNIT ( ) );
#4268 = EDGE_CURVE ( 'NONE', #4911, #8326, #16091, .T. ) ;
#4269 = AXIS2_PLACEMENT_3D ( 'NONE', #18071, #11210, #3248 ) ;
#4270 = CARTESIAN_POINT ( 'NONE',  ( 30.24348838687780727, 34.52875999999999834, -20.27293523655082552 ) ) ;
#4271 = DIRECTION ( 'NONE',  ( 0.000000000000000000, 1.000000000000000000, 0.000000000000000000 ) ) ;
#4272 = EDGE_CURVE ( 'NONE', #19184, #18464, #10245, .T. ) ;
#4273 = ORIENTED_EDGE ( 'NONE', *, *, #1727, .T. ) ;
#4274 = DIRECTION ( 'NONE',  ( 0.000000000000000000, 1.000000000000000000, 0.000000000000000000 ) ) ;
#4275 = CARTESIAN_POINT ( 'NONE',  ( 0.4312365985166283777, 18.52905954593687454, 1.381589547113361460 ) ) ;
#4276 = CIRCLE ( 'NONE', #5670, 1.983739999999999837 ) ;
#4277 = CARTESIAN_POINT ( 'NONE',  ( 20.04787453465361935, -2.740891176687007658, -14.09479187605280082 ) ) ;
#4278 = ORIENTED_EDGE ( 'NONE', *, *, #20989, .T. ) ;
#4279 = CARTESIAN_POINT ( 'NONE',  ( -22.90765545213488963, -10.87373999999999974, -9.869178565316103047 ) ) ;
#4280 = AXIS2_PLACEMENT_3D ( 'NONE', #4074, #4407, #11033 ) ;
#4281 = CARTESIAN_POINT ( 'NONE',  ( 8.505511374756364873, -6.752907499999998286, -20.97439202360551747 ) ) ;
#4282 = ORIENTED_EDGE ( 'NONE', *, *, #4842, .F. ) ;
#4283 = CARTESIAN_POINT ( 'NONE',  ( -17.46249999999999858, -1.983740000000001169, 0.000000000000000000 ) ) ;
#4284 = DIRECTION ( 'NONE',  ( 0.000000000000000000, 1.000000000000000000, 0.000000000000000000 ) ) ;
#4286 = DIRECTION ( 'NONE',  ( 0.000000000000000000, -1.000000000000000000, 0.000000000000000000 ) ) ;
#4285 = LINE ( 'NONE', #2406, #14814 ) ;
#4287 = AXIS2_PLACEMENT_3D ( 'NONE', #7337, #2016, #15538 ) ;
#4288 = ORIENTED_EDGE ( 'NONE', *, *, #12523, .T. ) ;
#4289 = VERTEX_POINT ( 'NONE', #17109 ) ;
#4290 = VECTOR ( 'NONE', #2611, 1000.000000000000000 ) ;
#4291 = CARTESIAN_POINT ( 'NONE',  ( 10.47583051940516619, -3.824893550810934517, -15.93653755199607147 ) ) ;
#4293 = CARTESIAN_POINT ( 'NONE',  ( 37.07154142533928365, -6.356984999999999886, -2.340318470350700508 ) ) ;
#4292 = CARTESIAN_POINT ( 'NONE',  ( 7.293525192738406382, 18.51518438473548045, 8.055948870987359456 ) ) ;
#4294 = VERTEX_POINT ( 'NONE', #293 ) ;
#4295 = CARTESIAN_POINT ( 'NONE',  ( 3.587117570992901960, 13.66083647730730277, -0.6928666555306400854 ) ) ;
#4296 = EDGE_CURVE ( 'NONE', #11391, #17636, #10137, .T. ) ;
#4297 = ORIENTED_EDGE ( 'NONE', *, *, #19624, .T. ) ;
#4298 = EDGE_CURVE ( 'NONE', #21044, #12158, #13171, .T. ) ;
#4299 = ORIENTED_EDGE ( 'NONE', *, *, #12848, .F. ) ;
#4300 = CIRCLE ( 'NONE', #16653, 1.190625000000000488 ) ;
#4301 = ORIENTED_EDGE ( 'NONE', *, *, #5314, .T. ) ;
#4302 = AXIS2_PLACEMENT_3D ( 'NONE', #15532, #8867, #15862 ) ;
#4303 = CIRCLE ( 'NONE', #18755, 0.5080000000000034488 ) ;
#4304 = CARTESIAN_POINT ( 'NONE',  ( 20.53156541068710439, -1.359447366214681985, -15.90722246059563361 ) ) ;
#4305 = DIRECTION ( 'NONE',  ( -0.1065921516619563053, -0.9937903127262235348, 0.03192064434796804129 ) ) ;
#4306 = DIRECTION ( 'NONE',  ( 0.000000000000000000, 1.000000000000000000, 0.000000000000000000 ) ) ;
#4307 = CARTESIAN_POINT ( 'NONE',  ( 28.97711086133420366, 30.56064500000000095, -10.71499000000000024 ) ) ;
#4308 = CARTESIAN_POINT ( 'NONE',  ( 2.122429293774134251, 11.85923521650776280, 1.930479901139369403 ) ) ;
#4309 = EDGE_LOOP ( 'NONE', ( #3331, #3538, #20402, #3851 ) ) ;
#4310 = CARTESIAN_POINT ( 'NONE',  ( 28.38195592936287781, 29.75832250000000201, -13.81504834214261024 ) ) ;
#4311 = DIRECTION ( 'NONE',  ( 0.000000000000000000, -1.000000000000000000, -0.000000000000000000 ) ) ;
#4312 = CARTESIAN_POINT ( 'NONE',  ( 29.76562500000000000, 32.54502000000000095, -4.317999999999999616 ) ) ;
#4313 = SURFACE_SIDE_STYLE ('',( #9710 ) ) ;
#4314 = DIRECTION ( 'NONE',  ( -1.000000000000000000, 0.000000000000000000, 0.000000000000000000 ) ) ;
#4315 = VERTEX_POINT ( 'NONE', #186 ) ;
#4316 = ORIENTED_EDGE ( 'NONE', *, *, #5859, .T. ) ;
#4317 = CARTESIAN_POINT ( 'NONE',  ( 8.572546314900550968, 11.84307591169006102, 5.427209531905369033 ) ) ;
#4319 = CARTESIAN_POINT ( 'NONE',  ( 12.76235139282079167, 21.25996874134203907, -20.69948241803004407 ) ) ;
#4318 = CARTESIAN_POINT ( 'NONE',  ( 28.97711086133420366, 30.56064500000000095, -10.31874999999999964 ) ) ;
#4320 = CARTESIAN_POINT ( 'NONE',  ( 13.37977302674483226, 14.47986448106203206, 6.886294595076251746 ) ) ;
#4321 = ORIENTED_EDGE ( 'NONE', *, *, #3212, .T. ) ;
#4322 = ORIENTED_EDGE ( 'NONE', *, *, #15590, .F. ) ;
#4323 = EDGE_CURVE ( 'NONE', #18042, #7386, #16783, .T. ) ;
#4324 = FACE_OUTER_BOUND ( 'NONE', #7605, .T. ) ;
#4325 = AXIS2_PLACEMENT_3D ( 'NONE', #1629, #21864, #15256 ) ;
#4326 = CARTESIAN_POINT ( 'NONE',  ( 7.324677171929614872, 13.28816258335607081, -1.995452644984494261 ) ) ;
#4327 = CARTESIAN_POINT ( 'NONE',  ( 4.264170397703306747, 12.02909395710813989, 2.247622554162475694 ) ) ;
#4328 = CARTESIAN_POINT ( 'NONE',  ( 6.422875249409071508, 19.96740888111275680, 0.2665559906438186299 ) ) ;
#4329 = VECTOR ( 'NONE', #20195, 1000.000000000000227 ) ;
#4330 = CIRCLE ( 'NONE', #19138, 30.16249999999998721 ) ;
#4331 = LINE ( 'NONE', #7641, #14625 ) ;
#4332 = CARTESIAN_POINT ( 'NONE',  ( 6.866916592308192513, 11.04801462030960124, 4.445165589993000488 ) ) ;
#4333 = CIRCLE ( 'NONE', #12454, 0.5079999999999965654 ) ;
#4334 = CARTESIAN_POINT ( 'NONE',  ( 13.61076747458670866, 21.46618676209390841, 1.782491636468937379 ) ) ;
#4335 = CARTESIAN_POINT ( 'NONE',  ( -16.73439918454169018, -4.609114529603660415, -25.92417111164088084 ) ) ;
#4336 = CARTESIAN_POINT ( 'NONE',  ( 4.569264072537790433, 10.97102203747262195, 3.822939839603590961 ) ) ;
#4337 = CARTESIAN_POINT ( 'NONE',  ( 1.470004468695772726, 12.67845410451087673, 8.026080939803462044 ) ) ;
#4338 = DIRECTION ( 'NONE',  ( -0.000000000000000000, -1.000000000000000000, 0.000000000000000000 ) ) ;
#4339 = CARTESIAN_POINT ( 'NONE',  ( 7.324228559365892899, 14.94885212140055408, 7.531391849507111047 ) ) ;
#4340 = CARTESIAN_POINT ( 'NONE',  ( 34.38097451710952868, 34.52875999999999834, 0.2081255904771098786 ) ) ;
#4341 = CARTESIAN_POINT ( 'NONE',  ( 59.65121809612895731, 32.54502000000000095, -2.485718937265306572 ) ) ;
#4342 = CARTESIAN_POINT ( 'NONE',  ( 15.97930640409513536, -8.428197996455596197, -14.86420790539115444 ) ) ;
#4343 = ORIENTED_EDGE ( 'NONE', *, *, #5346, .F. ) ;
#4344 = DIRECTION ( 'NONE',  ( 0.000000000000000000, -1.000000000000000000, -0.000000000000000000 ) ) ;
#4345 = AXIS2_PLACEMENT_3D ( 'NONE', #5326, #6661, #2008 ) ;
#4346 = CIRCLE ( 'NONE', #15297, 9.524999999999998579 ) ;
#4347 = CARTESIAN_POINT ( 'NONE',  ( 9.812260450953351310, 10.90820011318799132, 0.1177049192506583880 ) ) ;
#4348 = ORIENTED_EDGE ( 'NONE', *, *, #20281, .T. ) ;
#4349 = CARTESIAN_POINT ( 'NONE',  ( 20.47138736203545051, 0.6100621568841679832, 10.16364511138895921 ) ) ;
#4350 = ADVANCED_FACE ( 'NONE', ( #13693 ), #20393, .F. ) ;
#4351 = CARTESIAN_POINT ( 'NONE',  ( 5.607071462432890563, 12.48575941491167107, -0.5813519368072119775 ) ) ;
#4352 = FACE_BOUND ( 'NONE', #13992, .T. ) ;
#4353 = ORIENTED_EDGE ( 'NONE', *, *, #10760, .T. ) ;
#4354 = FACE_OUTER_BOUND ( 'NONE', #12868, .T. ) ;
#4355 = VECTOR ( 'NONE', #12247, 1000.000000000000000 ) ;
#4356 = CARTESIAN_POINT ( 'NONE',  ( 5.571415501051473207, 20.74427618698123510, 3.589970083868847528 ) ) ;
#4357 = CARTESIAN_POINT ( 'NONE',  ( 59.65121809612895731, 34.52875999999999834, -2.485718937265306572 ) ) ;
#4358 = EDGE_LOOP ( 'NONE', ( #16778, #1037, #12724, #5122, #12340, #21411 ) ) ;
#4359 = AXIS2_PLACEMENT_3D ( 'NONE', #1144, #11206, #14870 ) ;
#4360 = CARTESIAN_POINT ( 'NONE',  ( 7.721407704011980400, 16.36585256730476701, -2.399376772047163708 ) ) ;
#4361 = CARTESIAN_POINT ( 'NONE',  ( 29.36874999999999858, 9.921875000000000000, 8.731249999999999289 ) ) ;
#4362 = CARTESIAN_POINT ( 'NONE',  ( 53.92979111630304345, -6.519632010286108503, -15.65141968183250754 ) ) ;
#4363 = DIRECTION ( 'NONE',  ( 0.3928209820863022839, 0.000000000000000000, -0.9196149607486564515 ) ) ;
#4364 = EDGE_CURVE ( 'NONE', #8109, #13937, #15470, .T. ) ;
#4365 = CARTESIAN_POINT ( 'NONE',  ( 3.207890707543083586, 21.23115320172808040, 2.906853089031384840 ) ) ;
#4366 = VECTOR ( 'NONE', #13807, 1000.000000000000000 ) ;
#4367 = CARTESIAN_POINT ( 'NONE',  ( 17.22522857595987844, 36.51313500000000545, -15.04442098945225403 ) ) ;
#4368 = ORIENTED_EDGE ( 'NONE', *, *, #21688, .T. ) ;
#4369 = DIRECTION ( 'NONE',  ( 0.2490110332224850509, 0.000000000000000000, -0.9685006480810792739 ) ) ;
#4370 = CARTESIAN_POINT ( 'NONE',  ( 47.80475250345343596, 38.88803500000000213, -11.91473563638196786 ) ) ;
#4371 = ORIENTED_EDGE ( 'NONE', *, *, #17597, .F. ) ;
#4372 = EDGE_CURVE ( 'NONE', #16351, #21627, #12019, .T. ) ;
#4373 = CARTESIAN_POINT ( 'NONE',  ( 11.55108798147146310, 21.17147518458597943, 2.638599769568476194 ) ) ;
#4374 =( BOUNDED_CURVE ( )  B_SPLINE_CURVE ( 3, ( #2887, #14734, #6414, #21440 ),
 .UNSPECIFIED., .F., .F. ) 
 B_SPLINE_CURVE_WITH_KNOTS ( ( 4, 4 ),
 ( 0.1347261119420776476, 0.1486429212228488894 ),
 .UNSPECIFIED. ) 
 CURVE ( )  GEOMETRIC_REPRESENTATION_ITEM ( )  RATIONAL_B_SPLINE_CURVE ( ( 1.000000000000000000, 0.9999838602667434628, 0.9999838602667434628, 1.000000000000000000 ) ) 
 REPRESENTATION_ITEM ( '' )  );
#4375 = LINE ( 'NONE', #6015, #5260 ) ;
#4376 = AXIS2_PLACEMENT_3D ( 'NONE', #5533, #17263, #2109 ) ;
#4377 = CARTESIAN_POINT ( 'NONE',  ( 1.448403523286458494, 16.16488452566092349, 8.848146419262569395 ) ) ;
#4378 = EDGE_CURVE ( 'NONE', #20691, #5398, #18752, .T. ) ;
#4379 = EDGE_CURVE ( 'NONE', #20373, #9905, #1949, .T. ) ;
#4380 = CARTESIAN_POINT ( 'NONE',  ( 21.32767659074639255, -3.394316947765121384, -14.52283687711769566 ) ) ;
#4382 = DIRECTION ( 'NONE',  ( 0.000000000000000000, -1.000000000000000000, 0.000000000000000000 ) ) ;
#4381 = CARTESIAN_POINT ( 'NONE',  ( 4.859321299514149928, 12.65090407144326257, 7.048876997207147888 ) ) ;
#4383 = EDGE_LOOP ( 'NONE', ( #2871, #4348, #4906, #480, #6951, #21192 ) ) ;
#4384 = DIRECTION ( 'NONE',  ( 1.000000000000000000, 0.000000000000000000, 0.000000000000000000 ) ) ;
#4385 = CARTESIAN_POINT ( 'NONE',  ( 42.66304184606194383, 0.000000000000000000, -19.22597499813143784 ) ) ;
#4386 = EDGE_LOOP ( 'NONE', ( #19555, #18791, #19167, #15736 ) ) ;
#4387 = CARTESIAN_POINT ( 'NONE',  ( 20.11003911965812208, -1.207134136194158103, -14.79009638531434589 ) ) ;
#4388 = VECTOR ( 'NONE', #7512, 1000.000000000000000 ) ;
#4389 = CARTESIAN_POINT ( 'NONE',  ( 12.34467035336512808, -0.5412634058883231125, -16.55697708178870897 ) ) ;
#4390 = ORIENTED_EDGE ( 'NONE', *, *, #18333, .T. ) ;
#4391 = CARTESIAN_POINT ( 'NONE',  ( 9.347939006732550737, 17.21989818313373988, -2.888331931755111714 ) ) ;
#4392 = CARTESIAN_POINT ( 'NONE',  ( 52.79771328282338771, 34.52875999999999834, 3.317700572842066986 ) ) ;
#4393 = APPLICATION_CONTEXT ( 'automotive_design' ) ;
#4394 = CIRCLE ( 'NONE', #9320, 25.00312500000000426 ) ;
#4395 = ADVANCED_FACE ( 'NONE', ( #9916 ), #13370, .F. ) ;
#4396 = DIRECTION ( 'NONE',  ( 0.07875956036501312318, 0.000000000000000000, -0.9968936410927243807 ) ) ;
#4397 = PRODUCT_RELATED_PRODUCT_CATEGORY ( 'part', '', ( #14278 ) ) ;
#4398 = ORIENTED_EDGE ( 'NONE', *, *, #12330, .T. ) ;
#4399 = DIRECTION ( 'NONE',  ( 0.000000000000000000, -1.000000000000000000, 0.000000000000000000 ) ) ;
#4401 = DIRECTION ( 'NONE',  ( -0.9685006480810794960, 0.000000000000000000, -0.2490110332224836354 ) ) ;
#4400 = CYLINDRICAL_SURFACE ( 'NONE', #11987, 16.66875000000000284 ) ;
#4402 = VECTOR ( 'NONE', #9805, 1000.000000000000114 ) ;
#4403 = ORIENTED_EDGE ( 'NONE', *, *, #14971, .F. ) ;
#4404 = VERTEX_POINT ( 'NONE', #18434 ) ;
#4405 = EDGE_CURVE ( 'NONE', #18389, #12286, #7678, .T. ) ;
#4407 = DIRECTION ( 'NONE',  ( 0.000000000000000000, 1.000000000000000000, 0.000000000000000000 ) ) ;
#4406 = CARTESIAN_POINT ( 'NONE',  ( 1.170218911684995478, 11.63698894629814085, 6.546186411866827370 ) ) ;
#4408 = VERTEX_POINT ( 'NONE', #3306 ) ;
#4409 = CARTESIAN_POINT ( 'NONE',  ( 4.083167597562495033, 19.59760028129526788, -0.3681794837021826194 ) ) ;
#4410 = ORIENTED_EDGE ( 'NONE', *, *, #19358, .F. ) ;
#4411 = ORIENTED_EDGE ( 'NONE', *, *, #19101, .F. ) ;
#4412 = AXIS2_PLACEMENT_3D ( 'NONE', #19274, #17516, #489 ) ;
#4413 = CARTESIAN_POINT ( 'NONE',  ( 1.062191812101273003, 12.47827038174564684, 6.250278051991300821 ) ) ;
#4414 = ORIENTED_EDGE ( 'NONE', *, *, #14225, .T. ) ;
#4415 = AXIS2_PLACEMENT_3D ( 'NONE', #13870, #18919, #353 ) ;
#4416 = CARTESIAN_POINT ( 'NONE',  ( -1.351150467732365579, 28.56769750000000130, -27.17319717629097653 ) ) ;
#4417 = EDGE_CURVE ( 'NONE', #19312, #21087, #5060, .T. ) ;
#4418 = CARTESIAN_POINT ( 'NONE',  ( 49.72033008250774344, 32.54502000000000095, -2.687827786179598277 ) ) ;
#4419 = DIRECTION ( 'NONE',  ( -0.9037041334408598692, -0.3596272420165190220, -0.2323512126103423059 ) ) ;
#4420 = CARTESIAN_POINT ( 'NONE',  ( 41.45112526417833010, 0.000000000000000000, 7.778260066349530710 ) ) ;
#4421 = CARTESIAN_POINT ( 'NONE',  ( 3.517454366401044918, 13.17929039423700743, 8.136532573000508251 ) ) ;
#4422 = EDGE_CURVE ( 'NONE', #12648, #8841, #11812, .T. ) ;
#4423 = ADVANCED_FACE ( 'NONE', ( #1732 ), #8472, .T. ) ;
#4424 = VERTEX_POINT ( 'NONE', #20625 ) ;
#4425 = DIRECTION ( 'NONE',  ( -0.6744690509234938514, 0.7360996206939018904, 0.05699866455150646993 ) ) ;
#4426 = DIRECTION ( 'NONE',  ( 0.000000000000000000, -1.000000000000000000, -0.000000000000000000 ) ) ;
#4427 = LINE ( 'NONE', #11261, #11021 ) ;
#4428 = DIRECTION ( 'NONE',  ( 0.000000000000000000, 0.000000000000000000, -1.000000000000000000 ) ) ;
#4429 = EDGE_LOOP ( 'NONE', ( #11195, #7844, #18649, #2353 ) ) ;
#4430 = VERTEX_POINT ( 'NONE', #10580 ) ;
#4431 = CARTESIAN_POINT ( 'NONE',  ( 10.40657903342879997, 11.56703545653052068, 4.000892017491787911 ) ) ;
#4433 = DIRECTION ( 'NONE',  ( 0.000000000000000000, -1.000000000000000000, 0.000000000000000000 ) ) ;
#4432 = DIRECTION ( 'NONE',  ( 0.000000000000000000, 1.000000000000000000, 0.000000000000000000 ) ) ;
#4434 = CARTESIAN_POINT ( 'NONE',  ( 11.85443195533146010, 20.90808010024898067, -2.310623319762369121 ) ) ;
#4435 = ORIENTED_EDGE ( 'NONE', *, *, #21131, .T. ) ;
#4436 = AXIS2_PLACEMENT_3D ( 'NONE', #9704, #13158, #7722 ) ;
#4437 = ORIENTED_EDGE ( 'NONE', *, *, #1563, .T. ) ;
#4438 = DIRECTION ( 'NONE',  ( -0.9579671649362033747, 0.000000000000000000, 0.2868778675745011220 ) ) ;
#4439 = CARTESIAN_POINT ( 'NONE',  ( 7.947508136585422100, 20.23276147138264491, -1.405158123477003418 ) ) ;
#4440 = CARTESIAN_POINT ( 'NONE',  ( 6.703263711442990491, 20.44835075257027412, 0.9868673461823399551 ) ) ;
#4441 = CARTESIAN_POINT ( 'NONE',  ( 6.676020821304478936, 11.81234876462786687, 4.091397116453036276 ) ) ;
#4442 = DIRECTION ( 'NONE',  ( 0.000000000000000000, 1.000000000000000000, 0.000000000000000000 ) ) ;
#4443 = CARTESIAN_POINT ( 'NONE',  ( 7.812630522065525440, 11.33951387506710162, -0.1560246795265585462 ) ) ;
#4444 = AXIS2_PLACEMENT_3D ( 'NONE', #8216, #1676, #1468 ) ;
#4445 = CARTESIAN_POINT ( 'NONE',  ( 65.04486224192415023, 36.51313500000000545, -32.83524980818705785 ) ) ;
#4446 = DIRECTION ( 'NONE',  ( -0.000000000000000000, -1.000000000000000000, 0.000000000000000000 ) ) ;
#4447 = CARTESIAN_POINT ( 'NONE',  ( 7.496365336133834489, 16.64380874522678155, 8.500741285933822056 ) ) ;
#4448 = CARTESIAN_POINT ( 'NONE',  ( 1.627952902251037060, 13.66371438389476189, 8.848553374140269767 ) ) ;
#4449 = EDGE_CURVE ( 'NONE', #16972, #2587, #18537, .T. ) ;
#4450 = ORIENTED_EDGE ( 'NONE', *, *, #14838, .F. ) ;
#4451 = CARTESIAN_POINT ( 'NONE',  ( 2.463800489352728995, 20.09148914161242061, 6.261814795623706686 ) ) ;
#4452 = CARTESIAN_POINT ( 'NONE',  ( 52.91086381164393515, -1.983739999999999837, 3.812938856729753301 ) ) ;
#4453 = DIRECTION ( 'NONE',  ( -0.9964481331860212121, 0.000000000000000000, 0.08420877549337300871 ) ) ;
#4454 = CARTESIAN_POINT ( 'NONE',  ( 20.05076670763927282, -6.053556717652265995, -13.99866289979699197 ) ) ;
#4455 = ORIENTED_EDGE ( 'NONE', *, *, #3697, .T. ) ;
#4456 = DIRECTION ( 'NONE',  ( 0.000000000000000000, 1.000000000000000000, 0.000000000000000000 ) ) ;
#4457 = CARTESIAN_POINT ( 'NONE',  ( 9.081081133818898365, 14.53291942956394145, -3.329645429468344187 ) ) ;
#4458 = VERTEX_POINT ( 'NONE', #16313 ) ;
#4459 = CARTESIAN_POINT ( 'NONE',  ( 29.29500096977420043, 1.844679962977120002, 10.71104922697731965 ) ) ;
#4460 = CARTESIAN_POINT ( 'NONE',  ( 5.667851893490138515, 18.56944215186095803, -1.718953128397392671 ) ) ;
#4461 = DIRECTION ( 'NONE',  ( 0.000000000000000000, -1.000000000000000000, 0.000000000000000000 ) ) ;
#4462 = CARTESIAN_POINT ( 'NONE',  ( 4.441799159996215884, 19.87391983916490190, 6.423165949441382416 ) ) ;
#4463 = VERTEX_POINT ( 'NONE', #5486 ) ;
#4464 = CARTESIAN_POINT ( 'NONE',  ( 31.68988926855799448, 32.54502000000000095, 1.626235259850384418 ) ) ;
#4465 = CARTESIAN_POINT ( 'NONE',  ( 12.11879977990919421, 19.43893749999999798, 0.1373704394269426865 ) ) ;
#4466 = ORIENTED_EDGE ( 'NONE', *, *, #5218, .F. ) ;
#4467 = DIRECTION ( 'NONE',  ( 0.000000000000000000, 1.000000000000000000, 0.000000000000000000 ) ) ;
#4468 = CARTESIAN_POINT ( 'NONE',  ( 5.888305848254707264, 13.94198686298930134, -1.024452031420564957 ) ) ;
#4469 = CARTESIAN_POINT ( 'NONE',  ( 7.129426711373165304, 20.03265763155913959, 6.883267371180108007 ) ) ;
#4470 = DIRECTION ( 'NONE',  ( 0.000000000000000000, 1.000000000000000000, 0.000000000000000000 ) ) ;
#4471 = EDGE_CURVE ( 'NONE', #18470, #968, #21363, .T. ) ;
#4472 = DIRECTION ( 'NONE',  ( 0.1060008583745224581, 0.000000000000000000, 0.9943660382494288186 ) ) ;
#4473 = CARTESIAN_POINT ( 'NONE',  ( 20.53116362325268796, -1.359604737398370622, -15.90732750518314731 ) ) ;
#4474 = CARTESIAN_POINT ( 'NONE',  ( 12.25799425556778388, 34.52875999999999834, 0.2069032437451798767 ) ) ;
#4475 = ORIENTED_EDGE ( 'NONE', *, *, #8715, .F. ) ;
#4476 = DIRECTION ( 'NONE',  ( 0.000000000000000000, -1.000000000000000000, 0.000000000000000000 ) ) ;
#4477 = CARTESIAN_POINT ( 'NONE',  ( 47.80475250345343596, -6.356985000000002550, -11.91473563638196786 ) ) ;
#4478 = ORIENTED_EDGE ( 'NONE', *, *, #9450, .T. ) ;
#4479 = CARTESIAN_POINT ( 'NONE',  ( 11.38971108731577608, 21.23201434281770261, 2.202812224794820306 ) ) ;
#4480 = AXIS2_PLACEMENT_3D ( 'NONE', #6338, #11323, #14671 ) ;
#4481 = CARTESIAN_POINT ( 'NONE',  ( 1.434811090846531023, 16.35893803067423136, 8.856001068397819864 ) ) ;
#4482 = CARTESIAN_POINT ( 'NONE',  ( 13.97450013175296490, 2.289333815574723374, -16.08697015436425559 ) ) ;
#4483 = CARTESIAN_POINT ( 'NONE',  ( 59.52193197173441774, 0.000000000000000000, -3.260183413611184911 ) ) ;
#4484 = ORIENTED_EDGE ( 'NONE', *, *, #3484, .T. ) ;
#4485 =( LENGTH_UNIT ( ) NAMED_UNIT ( * ) SI_UNIT ( .MILLI., .METRE. ) );
#4486 = DIRECTION ( 'NONE',  ( 0.000000000000000000, 0.000000000000000000, 1.000000000000000000 ) ) ;
#4487 = PLANE ( 'NONE',  #4539 ) ;
#4488 = ORIENTED_EDGE ( 'NONE', *, *, #11302, .F. ) ;
#4489 = CARTESIAN_POINT ( 'NONE',  ( 19.38601130136307660, 0.1958779811795416381, -15.04182760293502241 ) ) ;
#4490 = ORIENTED_EDGE ( 'NONE', *, *, #4798, .T. ) ;
#4491 = CARTESIAN_POINT ( 'NONE',  ( 12.77710113932175062, 11.94611577877984132, 4.222729064079776329 ) ) ;
#4492 = CARTESIAN_POINT ( 'NONE',  ( 2.369555810156617426, 18.89992366948760250, 0.8526494300588405295 ) ) ;
#4493 = CARTESIAN_POINT ( 'NONE',  ( 11.64042750901279533, 20.25175440475918265, -3.155339158323879012 ) ) ;
#4494 = EDGE_CURVE ( 'NONE', #6613, #13482, #9434, .T. ) ;
#4495 = VECTOR ( 'NONE', #14829, 1000.000000000000000 ) ;
#4496 = EDGE_CURVE ( 'NONE', #20164, #1402, #7595, .T. ) ;
#4497 = DIRECTION ( 'NONE',  ( -0.8609107660235850723, 0.000000000000000000, 0.5087559856598092844 ) ) ;
#4498 = ORIENTED_EDGE ( 'NONE', *, *, #21150, .F. ) ;
#4499 = CARTESIAN_POINT ( 'NONE',  ( 42.94469661997857912, -76.79125307200000350, -18.48251861828712705 ) ) ;
#4500 = FACE_OUTER_BOUND ( 'NONE', #19320, .T. ) ;
#4501 = ORIENTED_EDGE ( 'NONE', *, *, #1116, .F. ) ;
#4502 = ORIENTED_EDGE ( 'NONE', *, *, #17880, .T. ) ;
#4503 = CARTESIAN_POINT ( 'NONE',  ( 20.47836239057684438, -0.2404636795067978394, -15.29125119441909497 ) ) ;
#4505 = DIRECTION ( 'NONE',  ( 0.000000000000000000, 1.000000000000000000, 0.000000000000000000 ) ) ;
#4504 = CARTESIAN_POINT ( 'NONE',  ( 1.989525294996288496, 11.82982598436980126, 1.785142876290339853 ) ) ;
#4506 = ORIENTED_EDGE ( 'NONE', *, *, #3973, .F. ) ;
#4507 = CARTESIAN_POINT ( 'NONE',  ( 4.204571555674638361, 19.96231018478896146, -0.06522048258607304749 ) ) ;
#4508 = ORIENTED_EDGE ( 'NONE', *, *, #9373, .T. ) ;
#4509 = VECTOR ( 'NONE', #17664, 1000.000000000000000 ) ;
#4510 = VERTEX_POINT ( 'NONE', #2053 ) ;
#4511 = EDGE_CURVE ( 'NONE', #6378, #624, #12988, .T. ) ;
#4512 = EDGE_LOOP ( 'NONE', ( #11655, #15104, #9971, #11088, #3272 ) ) ;
#4513 = B_SPLINE_CURVE_WITH_KNOTS ( 'NONE', 3,
 ( #16114, #10691, #7477, #17437, #15791, #2500, #14135, #5707, #12466, #19190, #4056, #4160, #10799, #17544, #2392, #10899, #9122, #14247, #17652, #20963, #9235, #4489, #9670, #16541, #18197, #21390, #2719, #17976, #3052, #16441, #9561, #4595, #14893, #8014, #8114, #16225, #18087, #16330, #7906, #1052, #11122, #4820, #11224, #12799, #18293, #4387, #2827, #1373, #11338, #17874, #6141, #9453, #13237, #1272 ),
 .UNSPECIFIED., .F., .F.,
 ( 4, 2, 2, 2, 2, 2, 2, 2, 2, 1, 2, 2, 2, 2, 2, 1, 1, 2, 2, 2, 2, 2, 2, 1, 2, 2, 2, 2, 4 ),
 ( 0.3951433275501288200, 0.4707511034793145921, 0.4896530474616097584, 0.4991040194527578411, 0.5038295054483319380, 0.5085549914439059238, 0.5180059634350532294, 0.5274569354262006460, 0.5463588794084951461, 0.5558098513996421186, 0.5605353373952158824, 0.5652608233907896462, 0.5841627673730825920, 0.6219666553376684837, 0.6408685993199608744, 0.6597705433022533761, 0.6975744312668370473, 0.7353783192314209405, 0.7542802632137127761, 0.7731822071960048337, 0.8487899831251725091, 0.8676919271074654549, 0.8771428990986118723, 0.8865938710897582897, 0.9243977590543427381, 0.9338487310454888224, 0.9432997030366349067, 0.9622016470189257431, 1.000005534983508193 ),
 .UNSPECIFIED. ) ;
#4514 = ADVANCED_FACE ( 'NONE', ( #1031 ), #14434, .F. ) ;
#4515 = CARTESIAN_POINT ( 'NONE',  ( 1.581041518826207692, -14.84248999999999974, -20.30277549736237575 ) ) ;
#4516 = CARTESIAN_POINT ( 'NONE',  ( 39.22866504299416590, 37.71595759399457393, -3.656247628902255631 ) ) ;
#4517 = DIRECTION ( 'NONE',  ( 0.9964481331860212121, 0.000000000000000000, -0.08420877549337300871 ) ) ;
#4518 = CARTESIAN_POINT ( 'NONE',  ( 29.98909767165928386, -6.754812500000002551, -5.214162619065493054 ) ) ;
#4519 = CARTESIAN_POINT ( 'NONE',  ( 2.884421797144688160, 11.35064653914199262, 5.241908264952396479 ) ) ;
#4520 = AXIS2_PLACEMENT_3D ( 'NONE', #20614, #5583, #398 ) ;
#4521 = VERTEX_POINT ( 'NONE', #408 ) ;
#4522 = CARTESIAN_POINT ( 'NONE',  ( 46.03750000000000142, -1.983739999999999393, -10.31874999999999964 ) ) ;
#4523 = CARTESIAN_POINT ( 'NONE',  ( 53.84486179190094646, -9.531985000000000596, -6.412645463410259872 ) ) ;
#4524 = CARTESIAN_POINT ( 'NONE',  ( -17.46249999999999858, 16.27314499999999953, 8.731249999999999289 ) ) ;
#4525 = DIRECTION ( 'NONE',  ( -0.000000000000000000, -1.000000000000000000, 0.000000000000000000 ) ) ;
#4526 = ORIENTED_EDGE ( 'NONE', *, *, #1137, .T. ) ;
#4527 = VERTEX_POINT ( 'NONE', #7162 ) ;
#4528 = CARTESIAN_POINT ( 'NONE',  ( 8.941343084498610594, 15.40389167150912009, -2.864627239135745462 ) ) ;
#4530 = DIRECTION ( 'NONE',  ( -0.4139637392816631345, 0.000000000000000000, 0.9102933716994446867 ) ) ;
#4529 = DIRECTION ( 'NONE',  ( 0.000000000000000000, 1.000000000000000000, 0.000000000000000000 ) ) ;
#4531 = CARTESIAN_POINT ( 'NONE',  ( 10.92162063437064923, 15.44784284617675674, -4.283584550483333864 ) ) ;
#4532 = ORIENTED_EDGE ( 'NONE', *, *, #18650, .F. ) ;
#4533 = VERTEX_POINT ( 'NONE', #1150 ) ;
#4534 = DIRECTION ( 'NONE',  ( 0.05085730733808393328, 0.000000000000000000, -0.9987059298363656357 ) ) ;
#4535 = EDGE_CURVE ( 'NONE', #699, #15950, #5127, .T. ) ;
#4536 = CARTESIAN_POINT ( 'NONE',  ( 6.309743394496731383, 19.72050476477846459, -0.01792138457645678709 ) ) ;
#4537 = EDGE_CURVE ( 'NONE', #20882, #16262, #7780, .T. ) ;
#4538 = EDGE_CURVE ( 'NONE', #16037, #2994, #7958, .T. ) ;
#4539 = AXIS2_PLACEMENT_3D ( 'NONE', #9015, #11336, #8338 ) ;
#4540 = CARTESIAN_POINT ( 'NONE',  ( 3.324034007969909332, 16.94026534804002537, 8.402710725375246881 ) ) ;
#4541 = LINE ( 'NONE', #14733, #6353 ) ;
#4542 = DIRECTION ( 'NONE',  ( 0.000000000000000000, 1.000000000000000000, 0.000000000000000000 ) ) ;
#4543 = LINE ( 'NONE', #19781, #12358 ) ;
#4544 = DIRECTION ( 'NONE',  ( -0.6702301885068628895, 0.000000000000000000, -0.7421532822901579785 ) ) ;
#4545 = CARTESIAN_POINT ( 'NONE',  ( 0.3942685348548155000, 11.70427427261698128, 3.243497937280782839 ) ) ;
#4546 = PLANE ( 'NONE',  #20369 ) ;
#4547 = ORIENTED_EDGE ( 'NONE', *, *, #15539, .T. ) ;
#4548 = CARTESIAN_POINT ( 'NONE',  ( 0.5010645890953140391, 18.57485916386803382, 1.285821070430232860 ) ) ;
#4549 = LINE ( 'NONE', #12865, #9875 ) ;
#4550 = CARTESIAN_POINT ( 'NONE',  ( 18.07371581377308800, -95.96551800000000298, -11.95909761906105473 ) ) ;
#4551 = CARTESIAN_POINT ( 'NONE',  ( 8.505511374756364873, 39.28205249999999893, -20.97439202360551747 ) ) ;
#4552 = ORIENTED_EDGE ( 'NONE', *, *, #18410, .F. ) ;
#4553 = DIRECTION ( 'NONE',  ( -1.000000000000000000, 0.000000000000000000, 0.000000000000000000 ) ) ;
#4554 = CARTESIAN_POINT ( 'NONE',  ( 5.241325608820580406, 15.44426253303012508, -2.166424616879202958 ) ) ;
#4555 = AXIS2_PLACEMENT_3D ( 'NONE', #12715, #16261, #11159 ) ;
#4556 = CARTESIAN_POINT ( 'NONE',  ( 10.55427167348027595, 21.69986197937489081, -0.09835946977028746374 ) ) ;
#4557 = ORIENTED_EDGE ( 'NONE', *, *, #9167, .T. ) ;
#4558 = B_SPLINE_SURFACE_WITH_KNOTS ( 'NONE', 3, 3, ( 
 ( #18092, #17877, #1376, #6357, #19842, #8018, #3054, #19526, #2831, #19950, #1275, #11229, #4716, #6032, #14899, #3153, #18203, #17979, #19623, #2723, #7696, #9778, #21174, #16545, #9880, #6247, #14788, #11556, #21288, #2949, #14687, #9565, #7801, #12804, #14576, #4824, #9457, #8119, #21618, #11456, #16228, #6477, #4391, #13129, #11125, #16445, #9677, #13241, #949, #14457, #1055, #6146, #12914, #4491, #7912, #16335, #11342, #1172, #21394, #13019, #19725, #4598, #11663, #15111, #3378, #20046, #17075 ),
 ( #5230, #13663, #15436, #5027, #1699, #16646, #1492, #15331, #8238, #11779, #8440, #1810, #15212, #12109, #16961, #264, #42, #11883, #18398, #1918, #155, #20364, #8555, #18719, #13344, #18510, #13772, #6899, #10109, #11991, #3702, #5132, #18832, #3591, #20476, #21830, #6682, #8663, #10330, #7005, #15012, #3274, #5345, #21728, #6580, #16856, #4917, #1599, #10006, #16760, #18612, #8341, #13444, #20152, #6794, #13552, #3478, #20260, #10214, #9095, #13895, #19276, #2255, #7565, #7343, #17625, #15543 ),
 ( #820, #7246, #5453, #17182, #4135, #8764, #10876, #5892, #15772, #2368, #21045, #8881, #12442, #8993, #5561, #17290, #375, #2138, #14327, #18937, #2477, #9206, #7447, #3808, #15990, #7127, #10776, #20595, #4032, #19169, #12653, #19381, #10443, #5797, #17519, #2021, #12217, #17415, #10544, #20812, #15874, #15664, #596, #491, #3921, #14004, #20706, #19045, #12319, #10666, #14109, #5679, #700, #20939, #14221, #3027, #14539, #11201, #4246, #10984, #2917, #17741, #21260, #17952, #11308, #2802, #21583 ),
 ( #11098, #9429, #14657, #21467, #1248, #4468, #7668, #1026, #7988, #21364, #6115, #9535, #19808, #12992, #13098, #21144, #1141, #12882, #19601, #5997, #16095, #9647, #13209, #6442, #4360, #16200, #16306, #9750, #925, #4683, #7882, #6220, #2697, #16414, #2589, #16513, #1345, #9322, #12770, #14429, #19697, #14865, #17851, #19494, #7772, #4570, #18057, #14761, #6325, #11426, #18173, #8090, #3560, #10300, #19919, #17045, #15303, #14983, #3126, #5109, #15185, #21696, #20338, #18585, #16929, #11858, #126 ),
 ( #8314, #3354, #13638, #6763, #6878, #6552, #16828, #15084, #6649, #13315, #9849, #3451, #6979, #15413, #20019, #9974, #13412, #18689, #16618, #5207, #1669, #4994, #18368, #10184, #240, #1892, #8637, #4792, #4889, #11525, #8407, #18267, #11633, #1461, #1573, #11, #21797, #10083, #13527, #3238, #8209, #1778, #16732, #20120, #11751, #18483, #11962, #20234, #8523, #20788, #13979, #10850, #20905, #20677, #9180, #5313, #17388, #5771, #12294, #14194, #7094, #2111, #347, #15518, #15847, #574, #18804 ),
 ( #15961, #675, #13861, #2337, #17159, #20565, #2453, #10635, #3674, #19250, #12525, #8852, #5536, #792, #3785, #10417, #13746, #12413, #17265, #20443, #467, #7319, #12077, #14080, #1999, #5425, #10518, #12190, #19019, #2229, #18914, #15635, #8966, #7219, #3895, #15745, #7421, #5653, #19141, #4007, #10748, #17493, #9072, #19350, #1519, #11584, #19974, #21228, #8263, #6504, #4845, #14928, #9911, #4218, #9404, #4940, #8148, #17827, #18320, #16784, #17927, #3300, #21643, #11691, #5968, #19461, #21750 ),
 ( #7642, #4332, #16173, #6604, #10958, #15036, #11175, #14510, #12738, #3178, #10034, #13367, #20074, #7540, #16070, #21020, #3080, #18431, #14403, #5867, #11073, #4443, #2672, #19577, #9802, #901, #14303, #13267, #12628, #17711, #2561, #9294, #16677, #21117, #998, #7747, #6084, #12857, #16569, #1405, #5591, #2285, #4166, #9351, #10908, #17774, #9024, #5713, #20843, #12473, #2621, #2506, #19197, #4062, #2401, #849, #10804, #14459, #14355, #5920, #12685, #4493, #21730, #8020, #1057, #16649, #9884 ),
 ( #20050, #13243, #18094, #7804, #21502, #3057, #15013, #1279, #6585, #4601, #6148, #9566, #19729, #14578, #11560, #2725, #6359, #21289, #21620, #8121, #1495, #21396, #2954, #11128, #17878, #9781, #9460, #6250, #9679, #18205, #16448, #13346, #11460, #8241, #14792, #13133, #12916, #16337, #19844, #16229, #11231, #19626, #19954, #17980, #11345, #13021, #4720, #16547, #2833, #1176, #4826, #14903, #1380, #6480, #7916, #14690, #18298, #3155, #1922, #5135, #8344, #1705, #8667, #15335, #15216, #10219, #20479 ),
 ( #1814, #45, #13558, #6688, #16763, #10335, #13901, #380, #5031, #16859, #20263, #3705, #1602, #5350, #8558, #11887, #3381, #17079, #7131, #10446, #17184, #4920, #13447, #18401, #160, #15549, #11782, #3276, #8445, #6903, #6798, #16965, #13667, #20155, #11665, #3594, #2024, #8767, #10010, #15116, #267, #21833, #18514, #11995, #18615, #10113, #12112, #3481, #20368, #5233, #15439, #18837, #7009, #13776, #14008, #8998, #7249, #497, #822, #7451, #3812, #5565, #5682, #2371, #928, #7569, #20710 ) ),
 .UNSPECIFIED., .F., .F., .F.,
 ( 4, 1, 1, 1, 1, 1, 4 ),
 ( 4, 1, 1, 1, 1, 1, 1, 1, 1, 1, 1, 1, 1, 1, 1, 1, 1, 1, 1, 1, 1, 1, 1, 1, 1, 1, 1, 1, 1, 1, 1, 1, 1, 1, 1, 1, 1, 1, 1, 1, 1, 1, 1, 1, 1, 1, 1, 1, 1, 1, 1, 1, 1, 1, 1, 1, 1, 1, 1, 1, 1, 1, 1, 1, 4 ),
 ( -0.01121212662510000062, 0.000000000000000000, 0.1250000000000000000, 0.2500000000000000000, 0.3750000000000000000, 0.5000000000000000000, 0.5112121266250999607 ),
 ( -0.02000000000000000042, -0.003749999999999999861, 0.01250000000000000069, 0.02875000000000000125, 0.04499999999999999833, 0.06124999999999999889, 0.07749999999999999944, 0.09375000000000000000, 0.1100000000000000006, 0.1262500000000000011, 0.1424999999999999878, 0.1587500000000000022, 0.1749999999999999889, 0.1912500000000000033, 0.2074999999999999900, 0.2237500000000000044, 0.2399999999999999911, 0.2562499999999999778, 0.2725000000000000200, 0.2887500000000000067, 0.3049999999999999933, 0.3212499999999999800, 0.3375000000000000222, 0.3537500000000000089, 0.3699999999999999956, 0.3862499999999999822, 0.4025000000000000244, 0.4187500000000000111, 0.4349999999999999978, 0.4512499999999999845, 0.4675000000000000266, 0.4837500000000000133, 0.5000000000000000000, 0.5162499999999999867, 0.5324999999999999734, 0.5487499999999999600, 0.5649999999999999467, 0.5812500000000000444, 0.5975000000000000311, 0.6137500000000000178, 0.6300000000000000044, 0.6462499999999999911, 0.6624999999999999778, 0.6787499999999999645, 0.6949999999999999512, 0.7112500000000000488, 0.7275000000000000355, 0.7437500000000000222, 0.7600000000000000089, 0.7762499999999999956, 0.7924999999999999822, 0.8087499999999999689, 0.8249999999999999556, 0.8412500000000000533, 0.8575000000000000400, 0.8737500000000000266, 0.8900000000000000133, 0.9062500000000000000, 0.9224999999999999867, 0.9387499999999999734, 0.9549999999999999600, 0.9712499999999999467, 0.9875000000000000444, 1.003749999999999920, 1.020000000000000018 ),
 .UNSPECIFIED. ) ;
#4559 = CARTESIAN_POINT ( 'NONE',  ( 28.90809283614979819, 1.647247860330810054, 10.68704647368243954 ) ) ;
#4560 = CARTESIAN_POINT ( 'NONE',  ( 8.305577890988885770, 21.07935306927017294, 5.301748380739248034 ) ) ;
#4561 = CARTESIAN_POINT ( 'NONE',  ( 19.79515554403045741, -3.968114999999999615, -10.69562145279641996 ) ) ;
#4562 = CARTESIAN_POINT ( 'NONE',  ( 1.342236859452698328, 13.15608644122636228, 7.515139044313254857 ) ) ;
#4563 = ADVANCED_FACE ( 'NONE', ( #2172 ), #5377, .T. ) ;
#4564 = CARTESIAN_POINT ( 'NONE',  ( 22.22454659879084460, -3.968114999999999615, -13.75904720189594244 ) ) ;
#4565 = CARTESIAN_POINT ( 'NONE',  ( 6.748805940682723659, 19.22513578221937891, 6.619665475902611007 ) ) ;
#4566 = EDGE_CURVE ( 'NONE', #7945, #16183, #10419, .T. ) ;
#4567 = DIRECTION ( 'NONE',  ( -0.8741107132214044340, 0.000000000000000000, -0.4857267349359799535 ) ) ;
#4568 = ORIENTED_EDGE ( 'NONE', *, *, #15488, .F. ) ;
#4569 = AXIS2_PLACEMENT_3D ( 'NONE', #20852, #12585, #4171 ) ;
#4570 = CARTESIAN_POINT ( 'NONE',  ( 10.97561116649450241, 21.20110815220486344, 0.1820916674951629788 ) ) ;
#4571 = LINE ( 'NONE', #7775, #10722 ) ;
#4572 = CARTESIAN_POINT ( 'NONE',  ( 38.55125416157952856, -5.304186826770175500, -4.427761586073884814 ) ) ;
#4573 = CARTESIAN_POINT ( 'NONE',  ( 0.4623469015994441933, 11.62092872259188070, 3.129209433992582223 ) ) ;
#4574 = LINE ( 'NONE', #19602, #14602 ) ;
#4575 = FACE_OUTER_BOUND ( 'NONE', #2758, .T. ) ;
#4576 = CARTESIAN_POINT ( 'NONE',  ( 6.763134108677117950, 11.26290425026184217, 2.704746052809542611 ) ) ;
#4577 = FACE_OUTER_BOUND ( 'NONE', #13450, .T. ) ;
#4578 = CARTESIAN_POINT ( 'NONE',  ( 21.23025279753435512, -3.527030707732595083, -15.02425900349073018 ) ) ;
#4579 = VECTOR ( 'NONE', #13637, 1000.000000000000227 ) ;
#4580 = FACE_BOUND ( 'NONE', #15338, .T. ) ;
#4581 = EDGE_LOOP ( 'NONE', ( #13433, #8731, #3861, #20771, #21272, #14746 ) ) ;
#4582 = DIRECTION ( 'NONE',  ( -0.9784543669157824697, 0.000000000000000000, -0.2064631973583561375 ) ) ;
#4583 = CARTESIAN_POINT ( 'NONE',  ( 9.058884679750676128, 36.51313500000000545, -16.32319115207028659 ) ) ;
#4584 = VERTEX_POINT ( 'NONE', #522 ) ;
#4585 = CARTESIAN_POINT ( 'NONE',  ( 10.69489229547795972, 21.01502399469208271, 0.3287616349347236011 ) ) ;
#4586 = LINE ( 'NONE', #7467, #6679 ) ;
#4587 = CARTESIAN_POINT ( 'NONE',  ( 20.36694164398600648, -3.336838402629868749, -14.76985127222394212 ) ) ;
#4588 = CYLINDRICAL_SURFACE ( 'NONE', #8158, 0.5080000000000006732 ) ;
#4589 = ORIENTED_EDGE ( 'NONE', *, *, #11647, .F. ) ;
#4590 =( NAMED_UNIT ( * ) PLANE_ANGLE_UNIT ( ) SI_UNIT ( $, .RADIAN. ) );
#4591 = DIRECTION ( 'NONE',  ( 1.000000000000000000, 0.000000000000000000, 0.000000000000000000 ) ) ;
#4592 = ADVANCED_FACE ( 'NONE', ( #7271 ), #14032, .T. ) ;
#4593 = EDGE_LOOP ( 'NONE', ( #8508, #9900 ) ) ;
#4594 = AXIS2_PLACEMENT_3D ( 'NONE', #1589, #9765, #21814 ) ;
#4595 = CARTESIAN_POINT ( 'NONE',  ( 19.67322075098676137, -0.4140642647013181854, -14.93818290753014821 ) ) ;
#4596 = CIRCLE ( 'NONE', #10586, 6.349999999999999645 ) ;
#4597 = VERTEX_POINT ( 'NONE', #19604 ) ;
#4598 = CARTESIAN_POINT ( 'NONE',  ( 11.69919614587864132, 19.71652463870320204, -2.532988136784334099 ) ) ;
#4599 = CARTESIAN_POINT ( 'NONE',  ( 2.473378706908319291, 19.20449835410846617, 1.096051056300948900 ) ) ;
#4600 = DIRECTION ( 'NONE',  ( -0.2490110332224857170, 0.000000000000000000, 0.9685006480810790519 ) ) ;
#4601 = CARTESIAN_POINT ( 'NONE',  ( 6.247691938729453831, 20.69450185495974281, -0.2536055519876236342 ) ) ;
#4602 = VECTOR ( 'NONE', #3550, 1000.000000000000000 ) ;
#4603 = CARTESIAN_POINT ( 'NONE',  ( 19.31280273682966353, -5.508750913041076558, -15.41181252894822862 ) ) ;
#4604 = DIRECTION ( 'NONE',  ( 1.000000000000000000, 0.000000000000000000, 0.000000000000000000 ) ) ;
#4605 = ORIENTED_EDGE ( 'NONE', *, *, #1413, .T. ) ;
#4606 = AXIS2_PLACEMENT_3D ( 'NONE', #15525, #683, #4226 ) ;
#4607 = DIRECTION ( 'NONE',  ( 0.000000000000000000, 1.000000000000000000, -0.000000000000000000 ) ) ;
#4608 = CARTESIAN_POINT ( 'NONE',  ( 1.268730000000000135, 8.334374999999999645, 10.71562499999999929 ) ) ;
#4609 = ORIENTED_EDGE ( 'NONE', *, *, #14486, .T. ) ;
#4610 = ORIENTED_EDGE ( 'NONE', *, *, #3116, .T. ) ;
#4611 = CARTESIAN_POINT ( 'NONE',  ( 20.33761533588227621, -6.627751949389748987, -15.08663078611084352 ) ) ;
#4613 = LINE ( 'NONE', #19965, #10633 ) ;
#4612 = CARTESIAN_POINT ( 'NONE',  ( 6.759686242205972029, 20.09752422452572418, 7.061613146868085167 ) ) ;
#4614 = ORIENTED_EDGE ( 'NONE', *, *, #10523, .F. ) ;
#4615 = CARTESIAN_POINT ( 'NONE',  ( 3.511489924716158395, 15.15732606925634762, -1.285905515786881947 ) ) ;
#4616 = ORIENTED_EDGE ( 'NONE', *, *, #4268, .F. ) ;
#4617 = EDGE_CURVE ( 'NONE', #13996, #12465, #8794, .T. ) ;
#4618 = AXIS2_PLACEMENT_3D ( 'NONE', #18657, #20409, #20528 ) ;
#4619 = ORIENTED_EDGE ( 'NONE', *, *, #665, .T. ) ;
#4620 = ORIENTED_EDGE ( 'NONE', *, *, #15180, .T. ) ;
#4621 = CARTESIAN_POINT ( 'NONE',  ( 2.356492409553436751, 12.28457074719288755, 2.882335299874351886 ) ) ;
#4622 = VECTOR ( 'NONE', #17750, 1000.000000000000000 ) ;
#4623 = CARTESIAN_POINT ( 'NONE',  ( 4.035585374492060673, 12.61491249240588530, 1.301411686255661726 ) ) ;
#4624 = DIRECTION ( 'NONE',  ( -0.5222415575336509797, 0.000000000000000000, -0.8527976052879290281 ) ) ;
#4625 = CARTESIAN_POINT ( 'NONE',  ( 39.39227298748875228, 37.79827878291772691, -3.494347496384869523 ) ) ;
#4626 = CYLINDRICAL_SURFACE ( 'NONE', #2266, 3.174999999999999378 ) ;
#4627 = CARTESIAN_POINT ( 'NONE',  ( 23.15492293361681320, 8.724202693596797786, -3.167564836549936480 ) ) ;
#4628 = CARTESIAN_POINT ( 'NONE',  ( 3.428905286597181856, 12.67427477258878810, 7.691402442796377414 ) ) ;
#4629 = AXIS2_PLACEMENT_3D ( 'NONE', #3525, #16010, #5912 ) ;
#4630 = EDGE_LOOP ( 'NONE', ( #7609, #5405, #11712, #17181, #14479, #11548 ) ) ;
#4631 = AXIS2_PLACEMENT_3D ( 'NONE', #10815, #20980, #17889 ) ;
#4632 = FACE_OUTER_BOUND ( 'NONE', #8935, .T. ) ;
#4633 = FACE_OUTER_BOUND ( 'NONE', #6159, .T. ) ;
#4634 = DIRECTION ( 'NONE',  ( -1.000000000000000000, 0.000000000000000000, 0.000000000000000000 ) ) ;
#4635 = CARTESIAN_POINT ( 'NONE',  ( 59.89111109153450485, 32.54502000000000095, -22.14529389979288965 ) ) ;
#4636 = EDGE_CURVE ( 'NONE', #17408, #12286, #16909, .T. ) ;
#4637 = CARTESIAN_POINT ( 'NONE',  ( 53.70914399163670083, 39.62082658259355838, -15.96531164363307376 ) ) ;
#4638 = ORIENTED_EDGE ( 'NONE', *, *, #7748, .F. ) ;
#4639 = EDGE_LOOP ( 'NONE', ( #9019, #17513, #15800, #10408 ) ) ;
#4640 = CARTESIAN_POINT ( 'NONE',  ( 8.218929569428507165, 20.70901284984930157, 0.2465254262590220458 ) ) ;
#4641 = FACE_OUTER_BOUND ( 'NONE', #11685, .T. ) ;
#4642 = CARTESIAN_POINT ( 'NONE',  ( 10.94240633158067411, 14.34350891603136091, -4.001608750109906687 ) ) ;
#4643 = ORIENTED_EDGE ( 'NONE', *, *, #3304, .F. ) ;
#4644 = ORIENTED_EDGE ( 'NONE', *, *, #7507, .F. ) ;
#4645 = CARTESIAN_POINT ( 'NONE',  ( -1.427050033073577806, 25.39269750000000059, -23.44038945102687066 ) ) ;
#4646 = EDGE_CURVE ( 'NONE', #15022, #6484, #2673, .T. ) ;
#4647 = EDGE_CURVE ( 'NONE', #3173, #17565, #10082, .T. ) ;
#4648 = ADVANCED_FACE ( 'NONE', ( #11760 ), #3033, .T. ) ;
#4649 = CARTESIAN_POINT ( 'NONE',  ( 8.109733825337782420, 20.49485801409760199, 4.711921892921808741 ) ) ;
#4650 = CARTESIAN_POINT ( 'NONE',  ( 6.949628868194021258, 12.30010770274149046, 5.335163355835638832 ) ) ;
#4651 = AXIS2_PLACEMENT_3D ( 'NONE', #9516, #8075, #16286 ) ;
#4652 = AXIS2_PLACEMENT_3D ( 'NONE', #14182, #10736, #7305 ) ;
#4653 = FACE_BOUND ( 'NONE', #5476, .T. ) ;
#4654 = CARTESIAN_POINT ( 'NONE',  ( 13.75689827559843970, 21.65865639734760251, 1.766977752662861390 ) ) ;
#4655 = CARTESIAN_POINT ( 'NONE',  ( 28.87608719841374949, -7.547927499999999235, -15.73691681567849976 ) ) ;
#4656 = CARTESIAN_POINT ( 'NONE',  ( 5.550539117013853385, 13.84493627167355179, 8.315640499742142921 ) ) ;
#4657 = CARTESIAN_POINT ( 'NONE',  ( 1.482627815308283026, 12.73650106816228700, 8.087698260707639974 ) ) ;
#4658 = CYLINDRICAL_SURFACE ( 'NONE', #20731, 4.365625000000000533 ) ;
#4659 = ORIENTED_EDGE ( 'NONE', *, *, #12053, .T. ) ;
#4660 = CARTESIAN_POINT ( 'NONE',  ( 0.5452244933112915248, 12.38707500932596162, 3.405961392030337542 ) ) ;
#4661 = CARTESIAN_POINT ( 'NONE',  ( 1.532169971477637782, 25.39269750000000059, -20.71839214105750315 ) ) ;
#4662 = DIRECTION ( 'NONE',  ( 0.9037041334408600912, 0.3596272420165190775, 0.2323512126103423614 ) ) ;
#4663 = CARTESIAN_POINT ( 'NONE',  ( 10.82333320179976432, -5.094404121093500493, -15.94728721271635585 ) ) ;
#4664 = ADVANCED_FACE ( 'NONE', ( #4577 ), #1352, .T. ) ;
#4665 = DIRECTION ( 'NONE',  ( -0.4080888115384288528, 0.000000000000000000, -0.9129422336036122632 ) ) ;
#4666 = CIRCLE ( 'NONE', #11019, 1.983739999999997838 ) ;
#4667 = ORIENTED_EDGE ( 'NONE', *, *, #1561, .T. ) ;
#4668 = LINE ( 'NONE', #1011, #7119 ) ;
#4669 = CIRCLE ( 'NONE', #15987, 0.3962400000000010358 ) ;
#4670 = AXIS2_PLACEMENT_3D ( 'NONE', #10593, #7051, #534 ) ;
#4671 = CARTESIAN_POINT ( 'NONE',  ( 13.58729491768447417, 22.20239475586336297, 2.426319669798093326 ) ) ;
#4672 = CARTESIAN_POINT ( 'NONE',  ( 9.410645419839852366, 11.94156677812711287, -1.622654999013667609 ) ) ;
#4673 = ORIENTED_EDGE ( 'NONE', *, *, #6673, .T. ) ;
#4674 = VECTOR ( 'NONE', #16688, 1000.000000000000114 ) ;
#4675 = CARTESIAN_POINT ( 'NONE',  ( 8.797223678989327666, 20.03400673711370672, 6.593457860109054103 ) ) ;
#4676 = AXIS2_PLACEMENT_3D ( 'NONE', #3655, #6745, #16716 ) ;
#4677 = DIRECTION ( 'NONE',  ( 0.000000000000000000, -1.000000000000000000, 0.000000000000000000 ) ) ;
#4678 = CARTESIAN_POINT ( 'NONE',  ( 1.089122662289458976, 12.39630382929348151, 6.275382864778182856 ) ) ;
#4679 = EDGE_CURVE ( 'NONE', #1990, #20092, #13998, .T. ) ;
#4680 = SURFACE_STYLE_USAGE ( .BOTH. , #19804 ) ;
#4681 =( REPRESENTATION_RELATIONSHIP ('NONE','NONE', #15554, #11018 ) REPRESENTATION_RELATIONSHIP_WITH_TRANSFORMATION ( #20931 )SHAPE_REPRESENTATION_RELATIONSHIP( ) );
#4682 = DIRECTION ( 'NONE',  ( 0.2868778675745010664, 0.000000000000000000, 0.9579671649362032637 ) ) ;
#4683 = CARTESIAN_POINT ( 'NONE',  ( 10.03171560225656478, 21.13787900135836395, 3.342723603854336645 ) ) ;
#4684 = CARTESIAN_POINT ( 'NONE',  ( 4.972972795178391081, 18.58281789573423026, 7.435623437359064170 ) ) ;
#4685 = CARTESIAN_POINT ( 'NONE',  ( 3.122592833242820554, 20.84690199368946040, 1.788550936533952251 ) ) ;
#4686 = DIRECTION ( 'NONE',  ( -0.5087559856598092844, 0.000000000000000000, -0.8609107660235850723 ) ) ;
#4687 = VECTOR ( 'NONE', #15000, 1000.000000000000114 ) ;
#4688 = CIRCLE ( 'NONE', #17414, 1.983739999999999393 ) ;
#4689 = CARTESIAN_POINT ( 'NONE',  ( 32.55306802826559220, 0.000000000000000000, -17.37731658638881527 ) ) ;
#4690 = CARTESIAN_POINT ( 'NONE',  ( 6.651328749655917250, 11.03939126535642146, 2.721905128854394285 ) ) ;
#4691 = FACE_OUTER_BOUND ( 'NONE', #17436, .T. ) ;
#4692 = CARTESIAN_POINT ( 'NONE',  ( 20.89888763844149366, -4.983212492264129878, -15.05476727860177455 ) ) ;
#4693 = EDGE_CURVE ( 'NONE', #8797, #6208, #19818, .T. ) ;
#4694 = EDGE_CURVE ( 'NONE', #16263, #18972, #554, .T. ) ;
#4695 = CARTESIAN_POINT ( 'NONE',  ( 13.48619406898445661, -14.84248999999999974, -16.00576350138265624 ) ) ;
#4696 = ORIENTED_EDGE ( 'NONE', *, *, #10338, .F. ) ;
#4697 = CARTESIAN_POINT ( 'NONE',  ( -17.46249999999999858, 0.000000000000000000, 0.000000000000000000 ) ) ;
#4698 = CARTESIAN_POINT ( 'NONE',  ( 10.95239689897913316, 12.51241342390697753, 5.072527772439351601 ) ) ;
#4699 = DIRECTION ( 'NONE',  ( 0.000000000000000000, 0.000000000000000000, -1.000000000000000000 ) ) ;
#4700 = VECTOR ( 'NONE', #8270, 1000.000000000000000 ) ;
#4701 = ORIENTED_EDGE ( 'NONE', *, *, #19356, .F. ) ;
#4702 = CARTESIAN_POINT ( 'NONE',  ( 9.558959319209352046, 18.22385816987663176, -2.518794820452257444 ) ) ;
#4703 = DIRECTION ( 'NONE',  ( -0.2490110332224855227, 0.000000000000000000, 0.9685006480810791629 ) ) ;
#4704 = FACE_OUTER_BOUND ( 'NONE', #14698, .T. ) ;
#4705 = CARTESIAN_POINT ( 'NONE',  ( 16.96554420789919604, 1.210820340708572029, -15.19753933136295032 ) ) ;
#4706 = CARTESIAN_POINT ( 'NONE',  ( 6.649638745689235186, 12.00122113815488056, 5.925618445732687256 ) ) ;
#4707 = EDGE_LOOP ( 'NONE', ( #3960, #4238, #8843, #749 ) ) ;
#4708 = DIRECTION ( 'NONE',  ( 1.000000000000000000, 0.000000000000000000, 0.000000000000000000 ) ) ;
#4709 = DIRECTION ( 'NONE',  ( 0.000000000000000000, 1.000000000000000000, 0.000000000000000000 ) ) ;
#4710 = CARTESIAN_POINT ( 'NONE',  ( 3.934324214432870281, 17.71509372232019075, -0.4743072054864678755 ) ) ;
#4711 = ORIENTED_EDGE ( 'NONE', *, *, #14121, .F. ) ;
#4712 = VECTOR ( 'NONE', #1028, 1000.000000000000000 ) ;
#4713 = LINE ( 'NONE', #21170, #4041 ) ;
#4714 = CARTESIAN_POINT ( 'NONE',  ( 20.11685381419291119, -5.681614476441408712, -14.67255263074746985 ) ) ;
#4715 = ORIENTED_EDGE ( 'NONE', *, *, #2919, .F. ) ;
#4716 = CARTESIAN_POINT ( 'NONE',  ( 8.089493120333704823, 20.59481639511846041, 4.745424403458926577 ) ) ;
#4717 = CARTESIAN_POINT ( 'NONE',  ( 2.901177870377362744, 20.07788797494241706, 2.155083431282422080 ) ) ;
#4718 = CIRCLE ( 'NONE', #15317, 2.381250000000001421 ) ;
#4719 = CARTESIAN_POINT ( 'NONE',  ( -3.845402119898529758, 26.98019749999999917, -31.39393985263922460 ) ) ;
#4720 = CARTESIAN_POINT ( 'NONE',  ( 11.30433373149261556, 22.16594858500680232, 2.034150544939726135 ) ) ;
#4721 = EDGE_CURVE ( 'NONE', #4510, #7810, #9856, .T. ) ;
#4722 = PLANE ( 'NONE',  #18717 ) ;
#4723 = AXIS2_PLACEMENT_3D ( 'NONE', #8206, #14979, #6551 ) ;
#4724 = ORIENTED_EDGE ( 'NONE', *, *, #3140, .T. ) ;
#4725 = CARTESIAN_POINT ( 'NONE',  ( 44.27024749654656688, -6.356984999999999886, -8.722764363618033201 ) ) ;
#4726 = DIRECTION ( 'NONE',  ( -0.3140771401027084853, 0.9459569826691583971, -0.08075231887918270235 ) ) ;
#4727 = ORIENTED_EDGE ( 'NONE', *, *, #5714, .T. ) ;
#4728 = ORIENTED_EDGE ( 'NONE', *, *, #21525, .T. ) ;
#4729 = FACE_OUTER_BOUND ( 'NONE', #15220, .T. ) ;
#4731 = DIRECTION ( 'NONE',  ( 0.000000000000000000, 0.000000000000000000, -1.000000000000000000 ) ) ;
#4730 = CARTESIAN_POINT ( 'NONE',  ( 3.389842854487740365, 15.44796252803982206, -1.429507839081749720 ) ) ;
#4732 = ORIENTED_EDGE ( 'NONE', *, *, #10056, .T. ) ;
#4733 = CARTESIAN_POINT ( 'NONE',  ( 5.431705152844418016, 21.53778799175918124, 3.212981151218359255 ) ) ;
#4734 = AXIS2_PLACEMENT_3D ( 'NONE', #10494, #20536, #17240 ) ;
#4735 = ORIENTED_EDGE ( 'NONE', *, *, #3420, .F. ) ;
#4736 = VERTEX_POINT ( 'NONE', #6658 ) ;
#4737 = CARTESIAN_POINT ( 'NONE',  ( 1.083593175512994611, 12.51931675915923137, 6.352092480932011398 ) ) ;
#4738 = CYLINDRICAL_SURFACE ( 'NONE', #10361, 0.7950200000000005041 ) ;
#4739 = ORIENTED_EDGE ( 'NONE', *, *, #20617, .F. ) ;
#4740 = VECTOR ( 'NONE', #21065, 1000.000000000000000 ) ;
#4741 = DIRECTION ( 'NONE',  ( -0.7421532822901579785, 0.000000000000000000, 0.6702301885068630005 ) ) ;
#4742 = AXIS2_PLACEMENT_3D ( 'NONE', #21048, #12557, #9433 ) ;
#4743 = DIRECTION ( 'NONE',  ( -0.000000000000000000, -1.000000000000000000, 0.000000000000000000 ) ) ;
#4744 = PRODUCT ( 'Handle Latch Pawl Plate', 'Handle Latch Pawl Plate', '', ( #7336 ) ) ;
#4745 = DIRECTION ( 'NONE',  ( -0.7334850928793775759, -0.6768732144311021548, 0.06198604769976992501 ) ) ;
#4746 = CARTESIAN_POINT ( 'NONE',  ( 1.893820563527240486, 18.08758566162994086, -0.4124606427257835328 ) ) ;
#4747 = EDGE_CURVE ( 'NONE', #10568, #19175, #14989, .T. ) ;
#4748 = ORIENTED_EDGE ( 'NONE', *, *, #4909, .T. ) ;
#4749 = CARTESIAN_POINT ( 'NONE',  ( -16.07247711516169275, 37.85422182005619618, -10.44681224123558039 ) ) ;
#4750 = DIRECTION ( 'NONE',  ( 0.000000000000000000, 1.000000000000000000, 0.000000000000000000 ) ) ;
#4751 = DIRECTION ( 'NONE',  ( 0.000000000000000000, 1.000000000000000000, 0.000000000000000000 ) ) ;
#4752 = CARTESIAN_POINT ( 'NONE',  ( 54.51779242482700027, 1.984375000000000000, -30.64740209392260084 ) ) ;
#4753 = ORIENTED_EDGE ( 'NONE', *, *, #9918, .T. ) ;
#4754 = EDGE_LOOP ( 'NONE', ( #6546, #13349, #13456, #21184 ) ) ;
#4755 = CARTESIAN_POINT ( 'NONE',  ( 10.60300064863796976, 14.29921781272587289, -3.573945592432405061 ) ) ;
#4756 = DIRECTION ( 'NONE',  ( 0.6702301885068632226, 0.000000000000000000, 0.7421532822901576454 ) ) ;
#4757 = AXIS2_PLACEMENT_3D ( 'NONE', #7560, #21043, #10982 ) ;
#4758 = ORIENTED_EDGE ( 'NONE', *, *, #11943, .T. ) ;
#4759 = VERTEX_POINT ( 'NONE', #9756 ) ;
#4760 = DIRECTION ( 'NONE',  ( 0.000000000000000000, 0.000000000000000000, -1.000000000000000000 ) ) ;
#4761 = CARTESIAN_POINT ( 'NONE',  ( 9.203126350871984940, 16.69853532098021986, 7.213164781469691533 ) ) ;
#4762 = AXIS2_PLACEMENT_3D ( 'NONE', #1869, #6625, #8386 ) ;
#4763 = CARTESIAN_POINT ( 'NONE',  ( 6.541934835182226848, 11.72101710144985276, 3.494563511944335232 ) ) ;
#4764 = ADVANCED_FACE ( 'NONE', ( #4691 ), #16519, .F. ) ;
#4765 = CARTESIAN_POINT ( 'NONE',  ( 52.49113927203492125, -7.547609999999999708, -16.14695822742135078 ) ) ;
#4766 = DIRECTION ( 'NONE',  ( 0.9685006480810792739, -0.000000000000000000, 0.2490110332224850509 ) ) ;
#4767 = CARTESIAN_POINT ( 'NONE',  ( 3.405894365792090817, 21.44911200421750053, 3.521272260944334764 ) ) ;
#4768 = CARTESIAN_POINT ( 'NONE',  ( 1.311185941550153222, 12.10675315277394759, 7.278560453910660755 ) ) ;
#4769 = EDGE_CURVE ( 'NONE', #138, #14162, #18556, .T. ) ;
#4770 = FACE_OUTER_BOUND ( 'NONE', #19525, .T. ) ;
#4771 = EDGE_CURVE ( 'NONE', #18623, #10280, #1579, .T. ) ;
#4772 = ORIENTED_EDGE ( 'NONE', *, *, #16413, .T. ) ;
#4773 = CARTESIAN_POINT ( 'NONE',  ( 5.184979831338328182, 12.95168332381294185, 6.668061790751404594 ) ) ;
#4774 = DIRECTION ( 'NONE',  ( 0.000000000000000000, -1.000000000000000000, 0.000000000000000000 ) ) ;
#4775 = DIRECTION ( 'NONE',  ( -0.8609107660235850723, 0.000000000000000000, 0.5087559856598092844 ) ) ;
#4776 = CARTESIAN_POINT ( 'NONE',  ( 19.40258015623733101, -6.852770372521438169, -14.12738853639282866 ) ) ;
#4777 = AXIS2_PLACEMENT_3D ( 'NONE', #7674, #2807, #4363 ) ;
#4778 = PLANE ( 'NONE',  #10177 ) ;
#4779 = ORIENTED_EDGE ( 'NONE', *, *, #11272, .F. ) ;
#4780 = CARTESIAN_POINT ( 'NONE',  ( 8.943237316433746642, 15.28165795756530265, -3.613428226286483191 ) ) ;
#4781 = DIRECTION ( 'NONE',  ( 0.000000000000000000, 1.000000000000000000, 0.000000000000000000 ) ) ;
#4782 = CARTESIAN_POINT ( 'NONE',  ( 9.219739506579587740, 12.92579275786359716, -2.519071767018113750 ) ) ;
#4783 = ORIENTED_EDGE ( 'NONE', *, *, #17214, .F. ) ;
#4784 = CARTESIAN_POINT ( 'NONE',  ( 8.663904165564538573, 20.38058929159417687, 6.250049521530280039 ) ) ;
#4785 = DIRECTION ( 'NONE',  ( 0.000000000000000000, 0.000000000000000000, 1.000000000000000000 ) ) ;
#4786 = CARTESIAN_POINT ( 'NONE',  ( 3.923274285735534939, 20.52844081774288298, 5.086198801183424933 ) ) ;
#4787 = CARTESIAN_POINT ( 'NONE',  ( 6.349023019544413060, 11.72897180233325187, 2.639096833093112604 ) ) ;
#4788 = DIRECTION ( 'NONE',  ( -0.2490110332224857170, 0.000000000000000000, 0.9685006480810790519 ) ) ;
#4789 = ORIENTED_EDGE ( 'NONE', *, *, #18705, .T. ) ;
#4790 = EDGE_CURVE ( 'NONE', #4315, #12696, #16834, .T. ) ;
#4791 = DIRECTION ( 'NONE',  ( -0.9784543669157944601, 0.000000000000000000, -0.2064631973582987945 ) ) ;
#4792 = CARTESIAN_POINT ( 'NONE',  ( 8.896463448791882556, 20.99150983053873887, -0.1081733280006275666 ) ) ;
#4793 = CARTESIAN_POINT ( 'NONE',  ( 5.334080576704635313, 14.09280588451894012, 7.447742775086575229 ) ) ;
#4794 = B_SPLINE_CURVE_WITH_KNOTS ( 'NONE', 3,
 ( #20118, #5206, #3558, #1569 ),
 .UNSPECIFIED., .F., .F.,
 ( 4, 4 ),
 ( 0.000000000000000000, 1.000000000000000000 ),
 .UNSPECIFIED. ) ;
#4795 = DIRECTION ( 'NONE',  ( 0.000000000000000000, 1.000000000000000000, 0.000000000000000000 ) ) ;
#4796 = CARTESIAN_POINT ( 'NONE',  ( -0.6273374921548363625, 20.81272068207762516, 3.698821178046660219 ) ) ;
#4797 = CARTESIAN_POINT ( 'NONE',  ( 17.30373842852263877, -3.968114999999999615, -12.15706637069277107 ) ) ;
#4798 = EDGE_CURVE ( 'NONE', #2743, #7667, #6226, .T. ) ;
#4799 = LINE ( 'NONE', #18178, #21271 ) ;
#4800 = LINE ( 'NONE', #11531, #2276 ) ;
#4801 = DIRECTION ( 'NONE',  ( -0.9685006480810791629, 0.000000000000000000, -0.2490110332224850231 ) ) ;
#4802 = CARTESIAN_POINT ( 'NONE',  ( 21.24987335672298627, -3.225771147898685243, -15.03024036818241527 ) ) ;
#4803 = CARTESIAN_POINT ( 'NONE',  ( -19.26602273594821924, -5.951855000000001006, -73.22163862549463431 ) ) ;
#4804 = ORIENTED_EDGE ( 'NONE', *, *, #18929, .T. ) ;
#4805 = DIRECTION ( 'NONE',  ( -0.000000000000000000, -1.000000000000000000, 0.000000000000000000 ) ) ;
#4806 = DIRECTION ( 'NONE',  ( -0.7421532822901579785, 0.000000000000000000, 0.6702301885068630005 ) ) ;
#4807 = ADVANCED_FACE ( 'NONE', ( #15091 ), #2319, .T. ) ;
#4808 = ORIENTED_EDGE ( 'NONE', *, *, #19973, .F. ) ;
#4809 = CARTESIAN_POINT ( 'NONE',  ( 13.04945465967934837, 13.27366431607636699, 5.426863059856754212 ) ) ;
#4810 = DIRECTION ( 'NONE',  ( -0.2868778675745010664, 0.000000000000000000, -0.9579671649362032637 ) ) ;
#4811 = FACE_OUTER_BOUND ( 'NONE', #4899, .T. ) ;
#4812 = CARTESIAN_POINT ( 'NONE',  ( 14.53774918468628208, -7.260662509237028495, -16.24585327058502315 ) ) ;
#4814 = DIRECTION ( 'NONE',  ( 0.6702301885068630005, 0.000000000000000000, 0.7421532822901579785 ) ) ;
#4813 = CARTESIAN_POINT ( 'NONE',  ( 0.1476213763842004201, 12.30129727290108121, 3.491265826091432878 ) ) ;
#4815 = EDGE_LOOP ( 'NONE', ( #20974, #6268, #21494, #3864 ) ) ;
#4816 = DIRECTION ( 'NONE',  ( 1.000000000000000000, 0.000000000000000000, 0.000000000000000000 ) ) ;
#4817 = DIRECTION ( 'NONE',  ( 1.000000000000000000, 0.000000000000000000, 0.000000000000000000 ) ) ;
#4818 = CARTESIAN_POINT ( 'NONE',  ( 4.087777094530046007, 18.47353267629715035, -0.1674047009188593116 ) ) ;
#4819 = VERTEX_POINT ( 'NONE', #21804 ) ;
#4820 = CARTESIAN_POINT ( 'NONE',  ( 19.98755129532091601, -0.9945011873913147671, -14.82825913642804849 ) ) ;
#4821 = ADVANCED_FACE ( 'NONE', ( #8530 ), #20575, .T. ) ;
#4822 = EDGE_CURVE ( 'NONE', #8026, #17335, #6768, .T. ) ;
#4823 = ORIENTED_EDGE ( 'NONE', *, *, #19349, .T. ) ;
#4824 = CARTESIAN_POINT ( 'NONE',  ( 10.98836716658659718, 12.61615142531242206, 5.351275285785762392 ) ) ;
#4825 = LINE ( 'NONE', #9678, #5680 ) ;
#4826 = CARTESIAN_POINT ( 'NONE',  ( 13.34863692440958793, 16.76855268369192586, 7.282520765264200335 ) ) ;
#4827 = CARTESIAN_POINT ( 'NONE',  ( 17.77073768271571197, -6.828400799270224475, -15.71113051208573808 ) ) ;
#4828 = DIRECTION ( 'NONE',  ( 0.000000000000000000, 1.000000000000000000, 0.000000000000000000 ) ) ;
#4829 = ORIENTED_EDGE ( 'NONE', *, *, #17099, .F. ) ;
#4830 = CARTESIAN_POINT ( 'NONE',  ( 10.29169076519744586, 20.23694724301938663, 4.892464605147674561 ) ) ;
#4831 = CARTESIAN_POINT ( 'NONE',  ( 11.49851465602529821, 15.66517251583919901, 7.649551592746075102 ) ) ;
#4832 = DIRECTION ( 'NONE',  ( 0.000000000000000000, 1.000000000000000000, 0.000000000000000000 ) ) ;
#4833 = EDGE_LOOP ( 'NONE', ( #209, #21241, #14980, #16450 ) ) ;
#4834 = VERTEX_POINT ( 'NONE', #5434 ) ;
#4835 = LINE ( 'NONE', #11570, #1734 ) ;
#4837 = CARTESIAN_POINT ( 'NONE',  ( 52.94929985906785674, 37.69729076100792753, -16.57396907547657605 ) ) ;
#4836 = CARTESIAN_POINT ( 'NONE',  ( 1.507113407974402630, 17.33792227738861058, 9.643085118255577015 ) ) ;
#4838 = ORIENTED_EDGE ( 'NONE', *, *, #16622, .T. ) ;
#4839 = CARTESIAN_POINT ( 'NONE',  ( 6.826301903410996630, 20.01283248996876196, 6.955117793078509081 ) ) ;
#4840 = ORIENTED_EDGE ( 'NONE', *, *, #8550, .F. ) ;
#4841 = EDGE_LOOP ( 'NONE', ( #17483, #13258, #15873, #9423 ) ) ;
#4842 = EDGE_CURVE ( 'NONE', #6814, #20045, #17165, .T. ) ;
#4843 = CARTESIAN_POINT ( 'NONE',  ( 70.64340948846358970, 74.97070807199999365, -10.53785647675949910 ) ) ;
#4844 = ORIENTED_EDGE ( 'NONE', *, *, #15319, .F. ) ;
#4845 = CARTESIAN_POINT ( 'NONE',  ( 13.63939561152206004, 16.76121402582646880, 7.104551226395147800 ) ) ;
#4846 = DIRECTION ( 'NONE',  ( 0.000000000000000000, 0.000000000000000000, -1.000000000000000000 ) ) ;
#4847 = CARTESIAN_POINT ( 'NONE',  ( 10.10534066920194185, 36.51313500000000545, -14.00784516691476966 ) ) ;
#4848 = DIRECTION ( 'NONE',  ( 0.000000000000000000, -1.000000000000000000, 0.000000000000000000 ) ) ;
#4849 = CARTESIAN_POINT ( 'NONE',  ( 1.716548453638899963, 16.68013709720543503, -0.6901774513339551387 ) ) ;
#4850 = ORIENTED_EDGE ( 'NONE', *, *, #20867, .F. ) ;
#4851 = DIRECTION ( 'NONE',  ( 0.7421532822901569793, 0.000000000000000000, -0.6702301885068642218 ) ) ;
#4852 = LINE ( 'NONE', #5163, #1835 ) ;
#4853 = CARTESIAN_POINT ( 'NONE',  ( -13.49374999999999858, 32.54502000000000095, 0.000000000000000000 ) ) ;
#4854 = CARTESIAN_POINT ( 'NONE',  ( 41.71184157647478230, 38.88803500000000213, -2.134205101306931862 ) ) ;
#4855 = ORIENTED_EDGE ( 'NONE', *, *, #20717, .F. ) ;
#4856 = ORIENTED_EDGE ( 'NONE', *, *, #16907, .T. ) ;
#4857 = CARTESIAN_POINT ( 'NONE',  ( 8.647516245636284182, 12.11223639541018215, 5.228518803211497534 ) ) ;
#4858 = VECTOR ( 'NONE', #894, 1000.000000000000227 ) ;
#4859 = DIRECTION ( 'NONE',  ( 0.000000000000000000, 1.000000000000000000, 0.000000000000000000 ) ) ;
#4860 = ORIENTED_EDGE ( 'NONE', *, *, #851, .T. ) ;
#4861 = VERTEX_POINT ( 'NONE', #5213 ) ;
#4862 = CARTESIAN_POINT ( 'NONE',  ( -2.028188046367890074, 23.41816500000000190, 0.3682158094503220069 ) ) ;
#4863 = ORIENTED_EDGE ( 'NONE', *, *, #6811, .F. ) ;
#4864 = CARTESIAN_POINT ( 'NONE',  ( 9.274122820243968945, 15.20243951512090597, 7.097396118508335405 ) ) ;
#4865 = ADVANCED_FACE ( 'NONE', ( #10644 ), #18921, .T. ) ;
#4866 = CARTESIAN_POINT ( 'NONE',  ( 1.952969610814715207, 8.739187247087119914, 8.731249999999999289 ) ) ;
#4867 = CARTESIAN_POINT ( 'NONE',  ( 3.648350219661197436, 14.72343274211524644, 9.065328312466423455 ) ) ;
#4868 = CARTESIAN_POINT ( 'NONE',  ( 0.08586711205702327043, 12.50995321353708079, 1.839738799454192275 ) ) ;
#4869 = CARTESIAN_POINT ( 'NONE',  ( 30.42699695299585017, -1.983739999999999393, -4.832012189960551041 ) ) ;
#4870 = EDGE_LOOP ( 'NONE', ( #21436, #318, #12492, #10388 ) ) ;
#4871 = CARTESIAN_POINT ( 'NONE',  ( 5.460367653841071700, 14.21946822237472752, 7.588426468924110324 ) ) ;
#4872 = DIRECTION ( 'NONE',  ( -0.9959941601142525691, 0.000000000000000000, -0.08941830359777946935 ) ) ;
#4873 = DIRECTION ( 'NONE',  ( -0.2490110332224850509, 0.000000000000000000, 0.9685006480810792739 ) ) ;
#4874 = FILL_AREA_STYLE_COLOUR ( '', #17745 ) ;
#4875 = EDGE_LOOP ( 'NONE', ( #20200, #15586, #17023, #4437 ) ) ;
#4876 = CARTESIAN_POINT ( 'NONE',  ( 10.82391557466618792, 14.15586088870902515, -4.040410652065021146 ) ) ;
#4877 = CARTESIAN_POINT ( 'NONE',  ( 17.30373842852263877, -1.983739999999999393, -12.15706637069277107 ) ) ;
#4878 = CARTESIAN_POINT ( 'NONE',  ( 9.501351411502088951, 19.27355507002826229, -2.869603047228580728 ) ) ;
#4879 = EDGE_LOOP ( 'NONE', ( #18763, #9909, #17672, #595 ) ) ;
#4880 = CARTESIAN_POINT ( 'NONE',  ( 9.179518564026135863, 18.59391849750369374, 7.516351665735313325 ) ) ;
#4881 = CYLINDRICAL_SURFACE ( 'NONE', #7395, 0.3962399999999999811 ) ;
#4882 = DIRECTION ( 'NONE',  ( 0.9784543669157820256, 0.000000000000000000, 0.2064631973583577473 ) ) ;
#4883 = CYLINDRICAL_SURFACE ( 'NONE', #5652, 1.190625000000000711 ) ;
#4884 = ADVANCED_FACE ( 'NONE', ( #20345 ), #246, .T. ) ;
#4885 = ADVANCED_FACE ( 'NONE', ( #20686 ), #12199, .F. ) ;
#4886 = DIRECTION ( 'NONE',  ( 0.2868778675745010664, 0.000000000000000000, 0.9579671649362032637 ) ) ;
#4887 = ORIENTED_EDGE ( 'NONE', *, *, #21733, .F. ) ;
#4888 = CARTESIAN_POINT ( 'NONE',  ( 53.95242430215955665, 38.88803500000000213, -23.51676380836238067 ) ) ;
#4889 = CARTESIAN_POINT ( 'NONE',  ( 9.524362993972204094, 21.55462128078298178, 1.594027096361315232 ) ) ;
#4890 = CARTESIAN_POINT ( 'NONE',  ( 5.297840055243947965, 11.43043024698558163, 5.501502898240879347 ) ) ;
#4891 = DIRECTION ( 'NONE',  ( 0.000000000000000000, 1.000000000000000000, 0.000000000000000000 ) ) ;
#4892 = CARTESIAN_POINT ( 'NONE',  ( -0.8970842057359728061, 34.12394749999999988, -22.54358764576276286 ) ) ;
#4893 = DIRECTION ( 'NONE',  ( -0.9579671649362034858, -3.931712979385797282E-31, 0.2868778675745011220 ) ) ;
#4894 = CARTESIAN_POINT ( 'NONE',  ( 2.915917464538113180, -3.968114999999999615, -18.72348548116188027 ) ) ;
#4895 = FACE_OUTER_BOUND ( 'NONE', #15046, .T. ) ;
#4896 = ORIENTED_EDGE ( 'NONE', *, *, #15769, .F. ) ;
#4897 = DIRECTION ( 'NONE',  ( 0.000000000000000000, 1.000000000000000000, 0.000000000000000000 ) ) ;
#4898 = EDGE_CURVE ( 'NONE', #699, #19423, #17273, .T. ) ;
#4899 = EDGE_LOOP ( 'NONE', ( #7893, #13735, #19720, #202 ) ) ;
#4900 = CARTESIAN_POINT ( 'NONE',  ( 12.96002489183415562, 12.72746115195602101, 4.972234354664247569 ) ) ;
#4901 = DIRECTION ( 'NONE',  ( -0.9579671649362032637, 0.000000000000000000, 0.2868778675745010664 ) ) ;
#4902 = DIRECTION ( 'NONE',  ( -0.000000000000000000, -1.000000000000000000, 0.000000000000000000 ) ) ;
#4903 = CARTESIAN_POINT ( 'NONE',  ( 19.10022651896773027, -0.1605816450576252885, -14.01190017167833091 ) ) ;
#4905 = DIRECTION ( 'NONE',  ( 0.000000000000000000, -1.000000000000000000, -0.000000000000000000 ) ) ;
#4904 = CARTESIAN_POINT ( 'NONE',  ( -0.07563368751253243816, 20.26160593876955929, 6.296573392346809683 ) ) ;
#4906 = ORIENTED_EDGE ( 'NONE', *, *, #17122, .T. ) ;
#4907 = CARTESIAN_POINT ( 'NONE',  ( 0.000000000000000000, 0.000000000000000000, 0.000000000000000000 ) ) ;
#4908 = FACE_OUTER_BOUND ( 'NONE', #5525, .T. ) ;
#4909 = EDGE_CURVE ( 'NONE', #7279, #21761, #16464, .T. ) ;
#4910 = AXIS2_PLACEMENT_3D ( 'NONE', #302, #15700, #15476 ) ;
#4911 = VERTEX_POINT ( 'NONE', #3791 ) ;
#4912 = EDGE_CURVE ( 'NONE', #13662, #20882, #6906, .T. ) ;
#4913 = CARTESIAN_POINT ( 'NONE',  ( 6.007537124480966995, 11.30044911324893242, 2.933760949667521434 ) ) ;
#4914 = PRODUCT ( 'Ratchet Operating Handle', 'Ratchet Operating Handle', '', ( #19040 ) ) ;
#4915 = CARTESIAN_POINT ( 'NONE',  ( 20.30414312236064234, -2.730712048100304656, -14.54529006522136569 ) ) ;
#4916 = ORIENTED_EDGE ( 'NONE', *, *, #8047, .T. ) ;
#4917 = CARTESIAN_POINT ( 'NONE',  ( 11.29207773696401240, 21.35684717879324168, 1.993224277495995844 ) ) ;
#4918 = VECTOR ( 'NONE', #6436, 1000.000000000000000 ) ;
#4919 = CARTESIAN_POINT ( 'NONE',  ( 24.99127163628573456, 23.80367230640320031, 2.964528152719008158 ) ) ;
#4920 = CARTESIAN_POINT ( 'NONE',  ( 7.696232935528439789, 11.34385124051986260, -0.1186037254217440495 ) ) ;
#4921 = CARTESIAN_POINT ( 'NONE',  ( 13.23439868007747222, -6.150278290301139705, -16.64446557221927137 ) ) ;
#4922 = CARTESIAN_POINT ( 'NONE',  ( 11.75439013559175017, -3.968114999999999615, 4.331204221326972359 ) ) ;
#4923 = ORIENTED_EDGE ( 'NONE', *, *, #20455, .F. ) ;
#4924 = CARTESIAN_POINT ( 'NONE',  ( 10.77485793864860497, 18.93952712132382032, 6.088229833558084003 ) ) ;
#4925 = CARTESIAN_POINT ( 'NONE',  ( 13.44644525748832287, 14.65557762784733598, 7.052608399104622450 ) ) ;
#4926 = ADVANCED_FACE ( 'NONE', ( #1787 ), #2120, .T. ) ;
#4927 = CARTESIAN_POINT ( 'NONE',  ( 0.05128277951103899640, 30.56064500000000095, 8.896810487299289250 ) ) ;
#4928 = VERTEX_POINT ( 'NONE', #15526 ) ;
#4929 = ORIENTED_EDGE ( 'NONE', *, *, #19106, .T. ) ;
#4930 = CARTESIAN_POINT ( 'NONE',  ( 12.02474915109715603, 34.52875999999999834, -13.51434638588835391 ) ) ;
#4932 = CARTESIAN_POINT ( 'NONE',  ( 29.45491884992628329, -3.968114999999999615, -15.58809351040512325 ) ) ;
#4931 = CARTESIAN_POINT ( 'NONE',  ( 2.384201206460603295, 20.83040400030756345, 6.653898520983334564 ) ) ;
#4933 = VERTEX_POINT ( 'NONE', #10309 ) ;
#4934 = CARTESIAN_POINT ( 'NONE',  ( 5.263634754952733807, 21.48398394320635063, 2.754189575719125926 ) ) ;
#4935 = ORIENTED_EDGE ( 'NONE', *, *, #6521, .F. ) ;
#4936 = ORIENTED_EDGE ( 'NONE', *, *, #8493, .F. ) ;
#4937 = DIRECTION ( 'NONE',  ( -0.9790635044817342925, 0.000000000000000000, 0.2035550397114870846 ) ) ;
#4938 = VERTEX_POINT ( 'NONE', #8860 ) ;
#4939 = CARTESIAN_POINT ( 'NONE',  ( 1.989949280992425962, 13.58121736296352644, 1.066273477831844341 ) ) ;
#4940 = CARTESIAN_POINT ( 'NONE',  ( 12.27481390375581149, 10.41612365926042116, 0.5751452393686051767 ) ) ;
#4941 = CARTESIAN_POINT ( 'NONE',  ( 4.322661532824636943, 12.01334099290857260, 2.632746656654277650 ) ) ;
#4942 = AXIS2_PLACEMENT_3D ( 'NONE', #6201, #18155, #16393 ) ;
#4943 = CARTESIAN_POINT ( 'NONE',  ( 37.29356535768673098, -6.356984999999999886, -6.700294045292300105 ) ) ;
#4944 = DIRECTION ( 'NONE',  ( -1.000000000000000000, 0.000000000000000000, 0.000000000000000000 ) ) ;
#4945 = CARTESIAN_POINT ( 'NONE',  ( 1.836581059345375300, 12.93351256954322182, 0.5952454918390250871 ) ) ;
#4946 = ORIENTED_EDGE ( 'NONE', *, *, #11522, .T. ) ;
#4947 = CARTESIAN_POINT ( 'NONE',  ( -22.69549233516161379, -1.587500000000002132, 1.149759107507315914 ) ) ;
#4948 = DIRECTION ( 'NONE',  ( 0.7532174416907910786, 0.000000000000000000, 0.6577716059034319773 ) ) ;
#4949 = CARTESIAN_POINT ( 'NONE',  ( 0.000000000000000000, 0.000000000000000000, 0.000000000000000000 ) ) ;
#4950 = ADVANCED_FACE ( 'NONE', ( #5543 ), #12301, .F. ) ;
#4951 = CARTESIAN_POINT ( 'NONE',  ( 53.83113913812347562, 39.20076143050763307, -15.79492098357274443 ) ) ;
#4952 = ORIENTED_EDGE ( 'NONE', *, *, #10578, .T. ) ;
#4953 = EDGE_CURVE ( 'NONE', #13623, #21520, #8312, .T. ) ;
#4954 = ORIENTED_EDGE ( 'NONE', *, *, #872, .T. ) ;
#4955 = CARTESIAN_POINT ( 'NONE',  ( 7.445348592948711541, 21.00148274865230036, 3.220760063665622397 ) ) ;
#4956 = AXIS2_PLACEMENT_3D ( 'NONE', #13094, #9745, #11306 ) ;
#4957 = CARTESIAN_POINT ( 'NONE',  ( 0.3054000514189714743, 20.95646860120554322, 6.387721792624859063 ) ) ;
#4958 = ORIENTED_EDGE ( 'NONE', *, *, #4081, .T. ) ;
#4959 = EDGE_LOOP ( 'NONE', ( #3713, #12711, #1289, #8359 ) ) ;
#4960 = CARTESIAN_POINT ( 'NONE',  ( 54.51779242482700027, 0.000000000000000000, -30.64740209392260084 ) ) ;
#4961 = ORIENTED_EDGE ( 'NONE', *, *, #4511, .F. ) ;
#4962 = VECTOR ( 'NONE', #5043, 1000.000000000000000 ) ;
#4963 = CARTESIAN_POINT ( 'NONE',  ( 9.205773807864597202, 13.78306251088634227, 6.508323188782061841 ) ) ;
#4964 = CARTESIAN_POINT ( 'NONE',  ( 61.65536943582333151, 34.52875999999999834, -11.98363747855214712 ) ) ;
#4965 = VECTOR ( 'NONE', #7835, 1000.000000000000000 ) ;
#4966 = VECTOR ( 'NONE', #4505, 1000.000000000000000 ) ;
#4967 = CARTESIAN_POINT ( 'NONE',  ( 48.60274532164483929, 38.88803500000000213, -11.03110938465478164 ) ) ;
#4968 = DIRECTION ( 'NONE',  ( 0.9579671649362032637, 0.000000000000000000, -0.2868778675745010664 ) ) ;
#4969 = DIRECTION ( 'NONE',  ( 0.9173788132826626862, 0.000000000000000000, -0.3980152169705242216 ) ) ;
#4970 = CARTESIAN_POINT ( 'NONE',  ( 0.6614644217660635706, 20.17319333280023130, 1.780821157163276602 ) ) ;
#4971 = CARTESIAN_POINT ( 'NONE',  ( 2.915917464538113180, 36.51313500000000545, -18.72348548116188027 ) ) ;
#4972 = EDGE_LOOP ( 'NONE', ( #6075, #12692, #4643, #4159 ) ) ;
#4973 = CARTESIAN_POINT ( 'NONE',  ( 6.069746319406092105, 12.28013972695870137, 0.9435336904642243061 ) ) ;
#4974 = CARTESIAN_POINT ( 'NONE',  ( 31.02798609601340729, 32.54502000000000095, -5.485920235548950252 ) ) ;
#4975 = DIRECTION ( 'NONE',  ( 0.6702301885068632226, 0.000000000000000000, 0.7421532822901576454 ) ) ;
#4976 = DIRECTION ( 'NONE',  ( 0.000000000000000000, -1.000000000000000000, -0.000000000000000000 ) ) ;
#4977 = AXIS2_PLACEMENT_3D ( 'NONE', #136, #2007, #15422 ) ;
#4978 = DIRECTION ( 'NONE',  ( -0.9964481331860212121, 0.000000000000000000, 0.08420877549337302259 ) ) ;
#4979 = ORIENTED_EDGE ( 'NONE', *, *, #6553, .T. ) ;
#4980 = ADVANCED_FACE ( 'NONE', ( #15644, #13872 ), #6984, .T. ) ;
#4981 = CARTESIAN_POINT ( 'NONE',  ( 7.437265405598497026, 11.41928500448566375, 0.003538791784208922958 ) ) ;
#4982 = DIRECTION ( 'NONE',  ( 0.2490110332224846346, 0.000000000000000000, -0.9685006480810792739 ) ) ;
#4983 = CARTESIAN_POINT ( 'NONE',  ( 12.49109536803858767, 20.73224863311122235, 5.227285940140482978 ) ) ;
#4984 = ORIENTED_EDGE ( 'NONE', *, *, #10953, .F. ) ;
#4985 = VECTOR ( 'NONE', #14323, 1000.000000000000000 ) ;
#4986 = AXIS2_PLACEMENT_3D ( 'NONE', #1389, #2960, #6487 ) ;
#4987 = CARTESIAN_POINT ( 'NONE',  ( 6.518464590081749499, 21.03009675402047307, 0.4263782151239406404 ) ) ;
#4988 = CARTESIAN_POINT ( 'NONE',  ( 1.268730000000000135, 8.334374999999999645, 8.731249999999999289 ) ) ;
#4989 = DIRECTION ( 'NONE',  ( 0.9488823340533149020, 0.2002559181063070792, 0.2439669719140961091 ) ) ;
#4990 = CARTESIAN_POINT ( 'NONE',  ( 6.554211239163197256, 19.72323599584319709, 6.144497509861348128 ) ) ;
#4991 = AXIS2_PLACEMENT_3D ( 'NONE', #13959, #3766, #7072 ) ;
#4992 = FACE_BOUND ( 'NONE', #11822, .T. ) ;
#4993 = VECTOR ( 'NONE', #13085, 1000.000000000000114 ) ;
#4994 = CARTESIAN_POINT ( 'NONE',  ( 8.201431583584922080, 11.69576222774042229, -0.06186996528689033686 ) ) ;
#4995 = CARTESIAN_POINT ( 'NONE',  ( 5.377269426412026654, 15.26854398707441263, 7.911424674534676349 ) ) ;
#4996 = VECTOR ( 'NONE', #8423, 1000.000000000000000 ) ;
#4997 = CARTESIAN_POINT ( 'NONE',  ( 0.8188405504440110505, 20.20188058797412012, 7.869697537972164980 ) ) ;
#4998 = DIRECTION ( 'NONE',  ( -0.9790635044817342925, 0.000000000000000000, 0.2035550397114870846 ) ) ;
#4999 = VECTOR ( 'NONE', #16604, 1000.000000000000114 ) ;
#5000 = AXIS2_PLACEMENT_3D ( 'NONE', #13880, #15651, #8352 ) ;
#5001 = DIRECTION ( 'NONE',  ( 1.000000000000000000, 0.000000000000000000, 0.000000000000000000 ) ) ;
#5002 = CARTESIAN_POINT ( 'NONE',  ( 0.01038544335751814124, 14.29169281587572371, 1.257015631361889652 ) ) ;
#5003 = CYLINDRICAL_SURFACE ( 'NONE', #4263, 30.16250000000000142 ) ;
#5004 = DIRECTION ( 'NONE',  ( 0.9037041334408598692, 0.3596272420165190220, 0.2323512126103423059 ) ) ;
#5005 = CARTESIAN_POINT ( 'NONE',  ( 17.27816767801022024, -8.264717885962401311, -15.79824796366183648 ) ) ;
#5006 = SURFACE_STYLE_USAGE ( .BOTH. , #11866 ) ;
#5007 = EDGE_CURVE ( 'NONE', #2509, #15569, #11146, .T. ) ;
#5008 = AXIS2_PLACEMENT_3D ( 'NONE', #1737, #19874, #21863 ) ;
#5009 = ORIENTED_EDGE ( 'NONE', *, *, #5352, .F. ) ;
#5010 = VECTOR ( 'NONE', #1875, 1000.000000000000000 ) ;
#5011 = CARTESIAN_POINT ( 'NONE',  ( 10.70434257023885749, 11.78744898684672648, 3.934915454683276081 ) ) ;
#5012 = DIRECTION ( 'NONE',  ( 0.000000000000000000, -1.000000000000000000, -0.000000000000000000 ) ) ;
#5013 = ORIENTED_EDGE ( 'NONE', *, *, #10687, .T. ) ;
#5014 = CARTESIAN_POINT ( 'NONE',  ( 12.43084882143255676, 11.33874016961500253, 2.586588179875889182 ) ) ;
#5015 = CARTESIAN_POINT ( 'NONE',  ( 14.73791976308111451, 19.43957250000000059, -17.32306410839158772 ) ) ;
#5016 = CARTESIAN_POINT ( 'NONE',  ( 19.78828714858439497, -5.681633152690531929, -13.39467244788724187 ) ) ;
#5018 = DIRECTION ( 'NONE',  ( 0.000000000000000000, 1.000000000000000000, 0.000000000000000000 ) ) ;
#5017 = CARTESIAN_POINT ( 'NONE',  ( 1.538271623210065053, 14.85629794888722266, 0.2443331916369595735 ) ) ;
#5019 = ORIENTED_EDGE ( 'NONE', *, *, #5849, .F. ) ;
#5020 = DIRECTION ( 'NONE',  ( 1.000000000000000000, 0.000000000000000000, 0.000000000000000000 ) ) ;
#5021 = FACE_OUTER_BOUND ( 'NONE', #21760, .T. ) ;
#5022 = AXIS2_PLACEMENT_3D ( 'NONE', #4919, #11559, #11458 ) ;
#5023 = CARTESIAN_POINT ( 'NONE',  ( 6.008293396711528622, 11.33814340415402100, 2.936286190031843546 ) ) ;
#5024 = CARTESIAN_POINT ( 'NONE',  ( 11.84474491476024482, -6.892609742072639989, -16.23866874929617055 ) ) ;
#5025 = ORIENTED_EDGE ( 'NONE', *, *, #16213, .T. ) ;
#5026 = CIRCLE ( 'NONE', #13182, 0.5080000000000022276 ) ;
#5027 = CARTESIAN_POINT ( 'NONE',  ( 6.099401774668048226, 11.87301092205614061, 1.618424562767362351 ) ) ;
#5028 = ADVANCED_FACE ( 'NONE', ( #2005 ), #12534, .T. ) ;
#5029 = CARTESIAN_POINT ( 'NONE',  ( 8.133926869846012764, 20.59418330540166053, 4.731814609752428957 ) ) ;
#5030 = DIRECTION ( 'NONE',  ( 0.000000000000000000, -1.000000000000000000, -0.000000000000000000 ) ) ;
#5031 = CARTESIAN_POINT ( 'NONE',  ( 5.748166118559234761, 19.23834655595790011, -1.494793178587818128 ) ) ;
#5032 = VECTOR ( 'NONE', #18373, 1000.000000000000000 ) ;
#5033 = CARTESIAN_POINT ( 'NONE',  ( 12.69010466362585987, -5.538311079261389658, -16.74561394863653163 ) ) ;
#5034 = EDGE_CURVE ( 'NONE', #21568, #12037, #19362, .T. ) ;
#5035 = ORIENTED_EDGE ( 'NONE', *, *, #10215, .T. ) ;
#5036 = ADVANCED_FACE ( 'NONE', ( #9079 ), #5661, .T. ) ;
#5037 = CARTESIAN_POINT ( 'NONE',  ( 8.430798958192390558, 20.36791151137297362, -0.04873577611252521286 ) ) ;
#5038 = CARTESIAN_POINT ( 'NONE',  ( 11.34324718026622136, 17.71682859275886557, 7.525604685906813529 ) ) ;
#5039 = CARTESIAN_POINT ( 'NONE',  ( 30.78626241496060700, 2.019535839764540430, -2.552201779827368622 ) ) ;
#5040 = ORIENTED_EDGE ( 'NONE', *, *, #4566, .F. ) ;
#5041 = ORIENTED_EDGE ( 'NONE', *, *, #4693, .F. ) ;
#5042 = CIRCLE ( 'NONE', #14600, 0.7950199999999993938 ) ;
#5043 = DIRECTION ( 'NONE',  ( 0.000000000000000000, -1.000000000000000000, 0.000000000000000000 ) ) ;
#5044 = CARTESIAN_POINT ( 'NONE',  ( 11.78095237921021621, 20.74046845656823734, -2.506342087363637727 ) ) ;
#5045 = CIRCLE ( 'NONE', #3999, 0.7950200000000003930 ) ;
#5047 = CARTESIAN_POINT ( 'NONE',  ( 70.64340948846358970, 30.56064500000000095, -10.53785647675949910 ) ) ;
#5046 = CARTESIAN_POINT ( 'NONE',  ( 0.3927195269979631975, 20.25378384025834322, 1.942505237861241740 ) ) ;
#5048 = VERTEX_POINT ( 'NONE', #6095 ) ;
#5049 = CARTESIAN_POINT ( 'NONE',  ( 6.562780996375648712, 20.62143860797926465, 6.272862003966319655 ) ) ;
#5050 = EDGE_LOOP ( 'NONE', ( #16753, #17727, #16544, #13146 ) ) ;
#5051 = CARTESIAN_POINT ( 'NONE',  ( 0.2130741384702063979, 13.20354400989074151, 2.231225264059853775 ) ) ;
#5052 = AXIS2_PLACEMENT_3D ( 'NONE', #12946, #10249, #4851 ) ;
#5053 = LINE ( 'NONE', #10237, #20589 ) ;
#5054 = ORIENTED_EDGE ( 'NONE', *, *, #9724, .F. ) ;
#5055 = EDGE_CURVE ( 'NONE', #17518, #12957, #20893, .T. ) ;
#5056 = VECTOR ( 'NONE', #20233, 1000.000000000000000 ) ;
#5057 =( GEOMETRIC_REPRESENTATION_CONTEXT ( 3 ) GLOBAL_UNCERTAINTY_ASSIGNED_CONTEXT ( ( #1926 ) ) GLOBAL_UNIT_ASSIGNED_CONTEXT ( ( #12674, #4590, #6136 ) ) REPRESENTATION_CONTEXT ( 'NONE', 'WORKASPACE' ) );
#5058 = DIRECTION ( 'NONE',  ( 0.000000000000000000, 1.000000000000000000, 0.000000000000000000 ) ) ;
#5059 = FACE_BOUND ( 'NONE', #2995, .T. ) ;
#5060 = LINE ( 'NONE', #21858, #11129 ) ;
#5061 = CARTESIAN_POINT ( 'NONE',  ( 1.762868328497313453, 17.14743653705518867, -0.6379456634701065054 ) ) ;
#5062 = EDGE_LOOP ( 'NONE', ( #79, #10861, #17128, #1742 ) ) ;
#5063 = ADVANCED_FACE ( 'NONE', ( #7756, #10966, #17837, #21238, #11184 ), #20916, .F. ) ;
#5064 = CARTESIAN_POINT ( 'NONE',  ( 50.99913033092320092, 1.984375000000000000, -7.029081061492260751 ) ) ;
#5065 = DIRECTION ( 'NONE',  ( 0.000000000000000000, 1.000000000000000000, 0.000000000000000000 ) ) ;
#5066 = FACE_BOUND ( 'NONE', #12798, .T. ) ;
#5067 = CARTESIAN_POINT ( 'NONE',  ( -12.30312499999999964, 2.380615000000000148, 8.731249999999999289 ) ) ;
#5069 = CARTESIAN_POINT ( 'NONE',  ( 14.68361992452378573, -7.115731319896963392, -15.13783436087320666 ) ) ;
#5068 = CARTESIAN_POINT ( 'NONE',  ( 46.03750000000000142, 0.000000000000000000, -10.31874999999999964 ) ) ;
#5070 = VECTOR ( 'NONE', #12144, 1000.000000000000000 ) ;
#5071 = ORIENTED_EDGE ( 'NONE', *, *, #1681, .T. ) ;
#5072 = ORIENTED_EDGE ( 'NONE', *, *, #3771, .T. ) ;
#5073 = CARTESIAN_POINT ( 'NONE',  ( 12.79864249265565412, 13.16814630638014272, 5.676106444755931513 ) ) ;
#5075 = CARTESIAN_POINT ( 'NONE',  ( 39.58386072796550081, 38.88803500000000213, -4.490541772578183100 ) ) ;
#5074 = FACE_OUTER_BOUND ( 'NONE', #9933, .T. ) ;
#5076 = ORIENTED_EDGE ( 'NONE', *, *, #18241, .T. ) ;
#5077 = ORIENTED_EDGE ( 'NONE', *, *, #7776, .F. ) ;
#5078 = DIRECTION ( 'NONE',  ( 0.000000000000000000, 1.000000000000000000, 0.000000000000000000 ) ) ;
#5079 = ORIENTED_EDGE ( 'NONE', *, *, #20823, .T. ) ;
#5080 = CARTESIAN_POINT ( 'NONE',  ( 9.016910062489662536, 12.61851657500311852, 5.516817133326245681 ) ) ;
#5081 = CARTESIAN_POINT ( 'NONE',  ( 66.79943102505561114, -1.983739999999999393, -12.07331878313145168 ) ) ;
#5082 = EDGE_CURVE ( 'NONE', #19124, #19591, #12749, .T. ) ;
#5083 = CIRCLE ( 'NONE', #12872, 3.970020000000002991 ) ;
#5084 = EDGE_CURVE ( 'NONE', #17030, #7588, #2174, .T. ) ;
#5085 = ADVANCED_FACE ( 'NONE', ( #582, #17719 ), #5978, .T. ) ;
#5086 = PLANE ( 'NONE',  #10746 ) ;
#5087 = FACE_OUTER_BOUND ( 'NONE', #2381, .T. ) ;
#5088 = CARTESIAN_POINT ( 'NONE',  ( -0.04318575428918173392, 17.49843205272302527, 0.1587271788072038559 ) ) ;
#5089 = CARTESIAN_POINT ( 'NONE',  ( 29.03861462519914838, 16.26393749999999727, -4.929525984831418128 ) ) ;
#5090 = ORIENTED_EDGE ( 'NONE', *, *, #14516, .F. ) ;
#5091 = CARTESIAN_POINT ( 'NONE',  ( 1.797397970145764079, 14.26529943814340129, 8.410342253699687021 ) ) ;
#5092 = AXIS2_PLACEMENT_3D ( 'NONE', #322, #17241, #20995 ) ;
#5093 = DIRECTION ( 'NONE',  ( 0.000000000000000000, 1.000000000000000000, 0.000000000000000000 ) ) ;
#5094 = CARTESIAN_POINT ( 'NONE',  ( 11.56192577415882816, 34.52875999999999834, 4.677561850332325299 ) ) ;
#5095 = DIRECTION ( 'NONE',  ( -0.2868778675745010664, 0.000000000000000000, -0.9579671649362032637 ) ) ;
#5096 = ORIENTED_EDGE ( 'NONE', *, *, #1116, .T. ) ;
#5097 = CARTESIAN_POINT ( 'NONE',  ( 6.928561174131742106, 14.40990712224419745, -2.484241094878467226 ) ) ;
#5098 = CARTESIAN_POINT ( 'NONE',  ( 10.89704555651259099, 21.97159967450292939, 0.8476583213610661138 ) ) ;
#5099 = ORIENTED_EDGE ( 'NONE', *, *, #8046, .F. ) ;
#5100 = CIRCLE ( 'NONE', #8265, 0.5079999999999996740 ) ;
#5101 = CARTESIAN_POINT ( 'NONE',  ( 9.317271201742652664, 12.75577108541303240, 6.731794365810285896 ) ) ;
#5102 = CARTESIAN_POINT ( 'NONE',  ( 5.388874681376627507, 14.21749487271361190, 7.613809980626520257 ) ) ;
#5103 = CARTESIAN_POINT ( 'NONE',  ( -22.70813868260604096, -1.587500000000002132, 1.090609736204201763 ) ) ;
#5104 = DIRECTION ( 'NONE',  ( 0.000000000000000000, 1.000000000000000000, 0.000000000000000000 ) ) ;
#5105 = CARTESIAN_POINT ( 'NONE',  ( 49.28028498622276032, 0.000000000000000000, -25.68670502218146368 ) ) ;
#5106 = AXIS2_PLACEMENT_3D ( 'NONE', #13338, #13659, #5228 ) ;
#5107 = EDGE_CURVE ( 'NONE', #12461, #13767, #15967, .T. ) ;
#5108 = PLANE ( 'NONE',  #12347 ) ;
#5109 = CARTESIAN_POINT ( 'NONE',  ( 11.41680985899818168, 16.27085401118786834, -3.868117637540980258 ) ) ;
#5110 = AXIS2_PLACEMENT_3D ( 'NONE', #13833, #8290, #15062 ) ;
#5111 = CARTESIAN_POINT ( 'NONE',  ( 2.556540001888353508, 11.20929286741210085, 3.415214070081132203 ) ) ;
#5112 = DIRECTION ( 'NONE',  ( 0.000000000000000000, -1.000000000000000000, -0.000000000000000000 ) ) ;
#5113 = CARTESIAN_POINT ( 'NONE',  ( 19.79101016780580125, -0.04868028894460403599, -14.86990150494959195 ) ) ;
#5114 = FACE_OUTER_BOUND ( 'NONE', #10650, .T. ) ;
#5115 = CARTESIAN_POINT ( 'NONE',  ( 10.72409186464204112, -4.809670885807078022, -15.96177715662992824 ) ) ;
#5116 = CARTESIAN_POINT ( 'NONE',  ( 10.02683081661366593, -14.84248999999999974, -16.89519978567464165 ) ) ;
#5117 = CARTESIAN_POINT ( 'NONE',  ( 19.58215480567678668, -6.970154277315572244, -15.30510421406360422 ) ) ;
#5118 = DIRECTION ( 'NONE',  ( -0.9129422336036514540, 0.000000000000000000, 0.4080888115383414783 ) ) ;
#5119 = EDGE_LOOP ( 'NONE', ( #3096, #6612, #11662, #3105 ) ) ;
#5120 = CARTESIAN_POINT ( 'NONE',  ( 9.966377742653406813, 21.56226365017680280, 4.095160954391674046 ) ) ;
#5121 = CARTESIAN_POINT ( 'NONE',  ( -2.256261688646920227, 9.924415000000001541, -0.3933872460174320240 ) ) ;
#5122 = ORIENTED_EDGE ( 'NONE', *, *, #9518, .T. ) ;
#5123 = CARTESIAN_POINT ( 'NONE',  ( 13.16814363374584040, 15.42447050205943171, 6.337326380791521885 ) ) ;
#5124 = CARTESIAN_POINT ( 'NONE',  ( 14.84133058652096082, -7.424716859588557760, -15.15897677154538670 ) ) ;
#5125 = CARTESIAN_POINT ( 'NONE',  ( 5.328913628694865068, 20.92139076675124443, 3.828052080691475290 ) ) ;
#5126 = ORIENTED_EDGE ( 'NONE', *, *, #13613, .F. ) ;
#5127 = CIRCLE ( 'NONE', #15398, 0.7950199999999993938 ) ;
#5128 = DIRECTION ( 'NONE',  ( 0.000000000000000000, -1.000000000000000000, 0.000000000000000000 ) ) ;
#5129 = DIRECTION ( 'NONE',  ( -0.9784543669157950152, 0.000000000000000000, -0.2064631973582961577 ) ) ;
#5130 = ADVANCED_FACE ( 'NONE', ( #7326 ), #5778, .F. ) ;
#5131 = ORIENTED_EDGE ( 'NONE', *, *, #11855, .F. ) ;
#5132 = CARTESIAN_POINT ( 'NONE',  ( 10.75030023683537195, 19.11233889549468046, 6.102107763926431616 ) ) ;
#5133 = CARTESIAN_POINT ( 'NONE',  ( 12.48890390579409804, 19.94235689841700321, 5.071047164889341374 ) ) ;
#5134 = CARTESIAN_POINT ( 'NONE',  ( 4.135937413354406900, 17.27089909971514103, -1.194672083787219785 ) ) ;
#5135 = CARTESIAN_POINT ( 'NONE',  ( 10.89370315683180479, 16.27139426067512318, -4.466024506084000478 ) ) ;
#5136 = AXIS2_PLACEMENT_3D ( 'NONE', #9983, #11640, #14873 ) ;
#5137 = CARTESIAN_POINT ( 'NONE',  ( 18.77364033892985518, -6.130631416302358083, -15.51152502305813563 ) ) ;
#5138 = CARTESIAN_POINT ( 'NONE',  ( 12.61411201210553124, 21.25996874134203907, -20.12292187596927562 ) ) ;
#5139 = ORIENTED_EDGE ( 'NONE', *, *, #691, .T. ) ;
#5140 = CARTESIAN_POINT ( 'NONE',  ( 10.96283612688636744, 18.09806758118428149, 6.499183517072732563 ) ) ;
#5141 = CARTESIAN_POINT ( 'NONE',  ( 9.495683531383955156, 19.32856220366442201, -2.983829338518813490 ) ) ;
#5142 = VERTEX_POINT ( 'NONE', #14522 ) ;
#5143 = ORIENTED_EDGE ( 'NONE', *, *, #2925, .T. ) ;
#5144 = CARTESIAN_POINT ( 'NONE',  ( -17.46249999999999858, 0.000000000000000000, 0.000000000000000000 ) ) ;
#5145 = CARTESIAN_POINT ( 'NONE',  ( 11.24603787521979292, 18.83455621386651657, -3.846526465982558651 ) ) ;
#5147 = DIRECTION ( 'NONE',  ( 0.000000000000000000, -1.000000000000000000, 0.000000000000000000 ) ) ;
#5146 = CARTESIAN_POINT ( 'NONE',  ( 1.612457752549369516, 18.21888756068997495, -0.2970092401833866469 ) ) ;
#5148 = ORIENTED_EDGE ( 'NONE', *, *, #7732, .T. ) ;
#5149 = CARTESIAN_POINT ( 'NONE',  ( 6.959724889100487921, 19.62783388037593113, 7.291040551301790629 ) ) ;
#5150 = CARTESIAN_POINT ( 'NONE',  ( 28.38195592936287781, 29.75832250000000201, -13.81504834214261024 ) ) ;
#5151 = ORIENTED_EDGE ( 'NONE', *, *, #12542, .F. ) ;
#5152 = CARTESIAN_POINT ( 'NONE',  ( 0.3312671956846478527, 12.76499037468851228, 2.828231451653164363 ) ) ;
#5153 = EDGE_CURVE ( 'NONE', #11670, #8981, #20794, .T. ) ;
#5154 = CARTESIAN_POINT ( 'NONE',  ( 9.256853431388732290, 36.51313500000000545, -17.09316853730597074 ) ) ;
#5155 = ORIENTED_EDGE ( 'NONE', *, *, #12493, .T. ) ;
#5156 = EDGE_CURVE ( 'NONE', #17362, #6011, #14089, .T. ) ;
#5157 = DIRECTION ( 'NONE',  ( 0.7421532822901569793, 0.000000000000000000, -0.6702301885068642218 ) ) ;
#5158 = CARTESIAN_POINT ( 'NONE',  ( -16.07247711516169275, 37.85422182005619618, -10.44681224123558039 ) ) ;
#5159 = CARTESIAN_POINT ( 'NONE',  ( 1.748847732169433122, 13.54295735595392713, 0.1347836150705659652 ) ) ;
#5160 = CARTESIAN_POINT ( 'NONE',  ( 46.03750000000000142, -1.983739999999999837, -10.31874999999999964 ) ) ;
#5161 = VERTEX_POINT ( 'NONE', #9187 ) ;
#5162 = DIRECTION ( 'NONE',  ( -0.7421532822901572013, 0.000000000000000000, 0.6702301885068637777 ) ) ;
#5163 = CARTESIAN_POINT ( 'NONE',  ( -16.88621914012359326, -3.266559801243759331, -10.37804376527844141 ) ) ;
#5164 =( LENGTH_UNIT ( ) NAMED_UNIT ( * ) SI_UNIT ( .MILLI., .METRE. ) );
#5165 = CARTESIAN_POINT ( 'NONE',  ( 65.51436440461340283, 30.56064500000000095, -12.87863775929475985 ) ) ;
#5167 = CARTESIAN_POINT ( 'NONE',  ( 19.79801356026766967, -2.842841826568478947, -14.18991051583819463 ) ) ;
#5166 = CARTESIAN_POINT ( 'NONE',  ( 50.62387473582167274, -1.983739999999999837, -28.41576006634952734 ) ) ;
#5168 = ORIENTED_EDGE ( 'NONE', *, *, #6705, .F. ) ;
#5169 = ORIENTED_EDGE ( 'NONE', *, *, #14023, .T. ) ;
#5170 = CARTESIAN_POINT ( 'NONE',  ( 11.29854319475162505, 11.62217351343478278, -0.9112959381959166993 ) ) ;
#5172 = LINE ( 'NONE', #18654, #8527 ) ;
#5171 = CARTESIAN_POINT ( 'NONE',  ( 1.893587539172431944, 21.28931287393832150, 4.984029115425525625 ) ) ;
#5173 = ORIENTED_EDGE ( 'NONE', *, *, #5084, .T. ) ;
#5174 = ADVANCED_FACE ( 'NONE', ( #801 ), #7548, .F. ) ;
#5175 = ORIENTED_EDGE ( 'NONE', *, *, #18024, .T. ) ;
#5176 = DIRECTION ( 'NONE',  ( 0.000000000000000000, 1.000000000000000000, 0.000000000000000000 ) ) ;
#5177 = VECTOR ( 'NONE', #1683, 1000.000000000000000 ) ;
#5178 = ORIENTED_EDGE ( 'NONE', *, *, #14926, .T. ) ;
#5179 = CARTESIAN_POINT ( 'NONE',  ( 7.441962019404808615, 15.55687304735987553, -2.062044669940330976 ) ) ;
#5180 = EDGE_CURVE ( 'NONE', #12537, #18019, #3953, .T. ) ;
#5181 = FACE_OUTER_BOUND ( 'NONE', #13236, .T. ) ;
#5182 = CARTESIAN_POINT ( 'NONE',  ( 24.71252020198295085, 8.768263569673496960, -0.7333271064221494884 ) ) ;
#5183 = DIRECTION ( 'NONE',  ( 0.000000000000000000, 1.000000000000000000, 0.000000000000000000 ) ) ;
#5184 = CARTESIAN_POINT ( 'NONE',  ( -0.1512147235091668429, 16.43876524939473427, 0.03898613886197917211 ) ) ;
#5185 = FACE_OUTER_BOUND ( 'NONE', #13037, .T. ) ;
#5186 = VECTOR ( 'NONE', #16992, 1000.000000000000000 ) ;
#5187 = ORIENTED_EDGE ( 'NONE', *, *, #12739, .T. ) ;
#5188 = CARTESIAN_POINT ( 'NONE',  ( 0.3131061926257734385, 14.25064834509208112, 1.086654584014467684 ) ) ;
#5189 = CARTESIAN_POINT ( 'NONE',  ( 48.60274532164400085, -6.356984999999999886, -11.03110938465571245 ) ) ;
#5190 = CARTESIAN_POINT ( 'NONE',  ( 8.505511374756364873, -6.752907499999998286, -20.97439202360551747 ) ) ;
#5191 = LINE ( 'NONE', #16914, #10313 ) ;
#5192 = EDGE_LOOP ( 'NONE', ( #7403, #19658, #6940, #9759 ) ) ;
#5193 = CARTESIAN_POINT ( 'NONE',  ( 7.904713968335747687, 21.25109391276654236, 5.115303111256516821 ) ) ;
#5194 = LINE ( 'NONE', #12283, #17725 ) ;
#5195 = CARTESIAN_POINT ( 'NONE',  ( 12.59241507530448700, 20.47534440713213399, 5.493007318766919056 ) ) ;
#5196 = VERTEX_POINT ( 'NONE', #7650 ) ;
#5197 = ADVANCED_FACE ( 'NONE', ( #11082 ), #14411, .F. ) ;
#5198 = ORIENTED_EDGE ( 'NONE', *, *, #2365, .T. ) ;
#5199 = EDGE_CURVE ( 'NONE', #6719, #9795, #1825, .T. ) ;
#5200 = DIRECTION ( 'NONE',  ( 0.000000000000000000, -1.000000000000000000, 0.000000000000000000 ) ) ;
#5201 = ADVANCED_FACE ( 'NONE', ( #13396 ), #8189, .T. ) ;
#5202 = CARTESIAN_POINT ( 'NONE',  ( 9.467427033990846397, 16.24499877588407415, 7.989881806620619642 ) ) ;
#5203 = CARTESIAN_POINT ( 'NONE',  ( 5.996572361146331076, 12.27647896852458231, 0.9633039103135406789 ) ) ;
#5204 = DIRECTION ( 'NONE',  ( -0.3140771401027084853, 0.9459569826691583971, -0.08075231887918270235 ) ) ;
#5205 = AXIS2_PLACEMENT_3D ( 'NONE', #11403, #9731, #11285 ) ;
#5206 = CARTESIAN_POINT ( 'NONE',  ( -15.84035234298375094, 34.98745120071231440, -10.46642885967841252 ) ) ;
#5207 = CARTESIAN_POINT ( 'NONE',  ( 9.028156031046822960, 11.14036371107460255, 3.487870285503237966 ) ) ;
#5208 = CARTESIAN_POINT ( 'NONE',  ( 1.849087750985239476, 21.29000687509540413, 4.997418387125741823 ) ) ;
#5209 = CARTESIAN_POINT ( 'NONE',  ( -15.27935546639805331, -3.968114999999999615, -26.04713531390440906 ) ) ;
#5210 = CARTESIAN_POINT ( 'NONE',  ( 20.02546805227182958, -0.5331770397073201107, -14.81556814719122528 ) ) ;
#5211 = CARTESIAN_POINT ( 'NONE',  ( 5.367523021788562332, 15.73778643695066393, 8.099033024334408637 ) ) ;
#5212 = FACE_OUTER_BOUND ( 'NONE', #12945, .T. ) ;
#5213 = CARTESIAN_POINT ( 'NONE',  ( 7.241402720468077092, 5.548947500000001476, -19.25049230170216319 ) ) ;
#5214 = CARTESIAN_POINT ( 'NONE',  ( 10.77549486952163171, -3.766819462804153584, -17.13936903969156589 ) ) ;
#5215 =( NAMED_UNIT ( * ) SI_UNIT ( $, .STERADIAN. ) SOLID_ANGLE_UNIT ( ) );
#5216 = VECTOR ( 'NONE', #9245, 1000.000000000000000 ) ;
#5217 = CARTESIAN_POINT ( 'NONE',  ( 10.57847960714909341, 20.55760711429452670, 5.741939694044305931 ) ) ;
#5218 = EDGE_CURVE ( 'NONE', #3856, #4078, #1807, .T. ) ;
#5219 = VERTEX_POINT ( 'NONE', #20003 ) ;
#5220 = EDGE_CURVE ( 'NONE', #18746, #1762, #15622, .T. ) ;
#5221 = CARTESIAN_POINT ( 'NONE',  ( 13.16825386439218804, 15.19382052832209240, 6.286146467198543419 ) ) ;
#5222 = CARTESIAN_POINT ( 'NONE',  ( 19.44050799006316055, -5.356675604303823945, -14.21729107038780704 ) ) ;
#5224 = CARTESIAN_POINT ( 'NONE',  ( 60.38511073144201191, 34.52875999999999834, -22.26373525985038526 ) ) ;
#5223 = CARTESIAN_POINT ( 'NONE',  ( 3.388451077024644320, 15.55943979790526122, -0.6790290128948724968 ) ) ;
#5225 = ORIENTED_EDGE ( 'NONE', *, *, #18561, .F. ) ;
#5226 = APPLICATION_PROTOCOL_DEFINITION ( 'draft international standard', 'automotive_design', 1998, #16121 ) ;
#5227 = DIRECTION ( 'NONE',  ( -0.1132953773954069598, 0.7241889112991808375, -0.6802312681817410667 ) ) ;
#5228 = DIRECTION ( 'NONE',  ( 0.2490110332224836354, 0.000000000000000000, -0.9685006480810794960 ) ) ;
#5229 = VERTEX_POINT ( 'NONE', #6307 ) ;
#5230 = CARTESIAN_POINT ( 'NONE',  ( 6.810114687682450096, 12.02592060257602213, 4.780769153879307787 ) ) ;
#5231 = CARTESIAN_POINT ( 'NONE',  ( 13.09416812643731909, 13.21983372403380130, 5.514055102800065278 ) ) ;
#5232 = CARTESIAN_POINT ( 'NONE',  ( 2.560652196950205184, 12.18301083390420203, 1.830247191258276729 ) ) ;
#5233 = CARTESIAN_POINT ( 'NONE',  ( 13.07015714027482822, 18.81087267297494137, 6.779469008999309487 ) ) ;
#5234 = DIRECTION ( 'NONE',  ( -0.3542738219355860418, 0.000000000000000000, -0.9351417320872557060 ) ) ;
#5235 = CARTESIAN_POINT ( 'NONE',  ( 16.61136152229415686, -7.189742716178133541, -15.95096700094411624 ) ) ;
#5236 = UNCERTAINTY_MEASURE_WITH_UNIT (LENGTH_MEASURE( 1.000000000000000082E-05 ), #6240, 'distance_accuracy_value', 'NONE');
#5237 = DIRECTION ( 'NONE',  ( 0.2490110332224869105, 8.271275069592406292E-16, -0.9685006480810787188 ) ) ;
#5238 = ORIENTED_EDGE ( 'NONE', *, *, #14198, .F. ) ;
#5239 = CARTESIAN_POINT ( 'NONE',  ( 8.869677037920350671, 20.91023519772625150, 1.107515482924187999 ) ) ;
#5240 = CARTESIAN_POINT ( 'NONE',  ( 10.97615036777638586, 19.57796819772926256, 6.726635352813386426 ) ) ;
#5241 = ORIENTED_EDGE ( 'NONE', *, *, #5502, .T. ) ;
#5242 = EDGE_CURVE ( 'NONE', #1819, #18960, #14205, .T. ) ;
#5243 = VECTOR ( 'NONE', #19413, 1000.000000000000114 ) ;
#5244 = DIRECTION ( 'NONE',  ( -0.2490110332224846346, 0.000000000000000000, 0.9685006480810792739 ) ) ;
#5245 = DIRECTION ( 'NONE',  ( 0.000000000000000000, 1.000000000000000000, 0.000000000000000000 ) ) ;
#5247 = DIRECTION ( 'NONE',  ( 0.000000000000000000, 1.000000000000000000, 0.000000000000000000 ) ) ;
#5246 = CARTESIAN_POINT ( 'NONE',  ( 5.901476864229157293, 11.26983891803934235, 1.171034228512400022 ) ) ;
#5248 = ORIENTED_EDGE ( 'NONE', *, *, #10848, .T. ) ;
#5249 = CARTESIAN_POINT ( 'NONE',  ( 6.720649448207257848, 11.03335150912079143, 4.237661643980517923 ) ) ;
#5250 = FACE_OUTER_BOUND ( 'NONE', #4879, .T. ) ;
#5251 = ORIENTED_EDGE ( 'NONE', *, *, #5180, .F. ) ;
#5252 = VECTOR ( 'NONE', #13091, 1000.000000000000114 ) ;
#5253 = LINE ( 'NONE', #20618, #6130 ) ;
#5254 = EDGE_LOOP ( 'NONE', ( #1062, #18163, #20420, #19240 ) ) ;
#5255 = DIRECTION ( 'NONE',  ( -0.9964481331860212121, 0.000000000000000000, 0.08420877549337302259 ) ) ;
#5256 = DIRECTION ( 'NONE',  ( -0.9790635044817341814, 0.000000000000000000, 0.2035550397114869736 ) ) ;
#5257 = CARTESIAN_POINT ( 'NONE',  ( 0.02083138522552824973, 12.30439499999999953, 7.210477125664100484 ) ) ;
#5258 = CARTESIAN_POINT ( 'NONE',  ( 4.901426570561191021, 19.87298744257788385, 7.435174622645311260 ) ) ;
#5259 = CARTESIAN_POINT ( 'NONE',  ( 55.56250000000000000, 0.000000000000000000, -10.31874999999999964 ) ) ;
#5260 = VECTOR ( 'NONE', #19510, 1000.000000000000000 ) ;
#5261 = EDGE_LOOP ( 'NONE', ( #21498, #11220, #12755, #15152 ) ) ;
#5262 = DIRECTION ( 'NONE',  ( -3.089352305546554052E-14, 1.000000000000000000, 2.257689246356112745E-14 ) ) ;
#5263 = CARTESIAN_POINT ( 'NONE',  ( 9.275488759993784527, -6.752907499999998286, -20.77642327197297689 ) ) ;
#5264 =( NAMED_UNIT ( * ) SI_UNIT ( $, .STERADIAN. ) SOLID_ANGLE_UNIT ( ) );
#5265 = AXIS2_PLACEMENT_3D ( 'NONE', #14840, #4442, #7854 ) ;
#5267 = CARTESIAN_POINT ( 'NONE',  ( 19.79304348009334547, -3.380154523412622236, -14.16596585955715781 ) ) ;
#5266 = DIRECTION ( 'NONE',  ( 0.000000000000000000, 1.000000000000000000, 0.000000000000000000 ) ) ;
#5268 = ORIENTED_EDGE ( 'NONE', *, *, #311, .T. ) ;
#5269 = ORIENTED_EDGE ( 'NONE', *, *, #573, .T. ) ;
#5270 = EDGE_CURVE ( 'NONE', #11600, #18667, #13140, .T. ) ;
#5271 = CARTESIAN_POINT ( 'NONE',  ( 11.94242217153389873, 20.96877941592346062, -1.128413410470644029 ) ) ;
#5273 = PLANE ( 'NONE',  #15273 ) ;
#5272 = CARTESIAN_POINT ( 'NONE',  ( 3.657526251337493761, 16.52265399103842825, 9.296182230382092015 ) ) ;
#5274 = EDGE_LOOP ( 'NONE', ( #11800, #3078, #13265, #12834 ) ) ;
#5275 = VERTEX_POINT ( 'NONE', #14850 ) ;
#5276 = DIRECTION ( 'NONE',  ( 0.000000000000000000, 1.000000000000000000, 0.000000000000000000 ) ) ;
#5277 = ORIENTED_EDGE ( 'NONE', *, *, #15492, .F. ) ;
#5278 = CARTESIAN_POINT ( 'NONE',  ( 7.652417843280233001, 12.83819351580675239, -0.6376004508967495488 ) ) ;
#5279 = ORIENTED_EDGE ( 'NONE', *, *, #2874, .T. ) ;
#5280 = CIRCLE ( 'NONE', #21169, 0.5953125000000005773 ) ;
#5281 = VECTOR ( 'NONE', #5569, 1000.000000000000000 ) ;
#5282 = EDGE_CURVE ( 'NONE', #4533, #1721, #9734, .T. ) ;
#5283 = CARTESIAN_POINT ( 'NONE',  ( -21.43124999999999858, 0.000000000000000000, -4.860316984116058095E-16 ) ) ;
#5284 = DIRECTION ( 'NONE',  ( 0.000000000000000000, 0.000000000000000000, 1.000000000000000000 ) ) ;
#5285 = CARTESIAN_POINT ( 'NONE',  ( 3.450345209542672098, 17.80254839864814542, 8.992318556635597204 ) ) ;
#5286 = CARTESIAN_POINT ( 'NONE',  ( 49.41195815393805901, 32.54502000000000805, -1.411525001868561224 ) ) ;
#5287 = VECTOR ( 'NONE', #3121, 1000.000000000000000 ) ;
#5288 = EDGE_LOOP ( 'NONE', ( #5396, #12812, #11337, #5076 ) ) ;
#5289 = CARTESIAN_POINT ( 'NONE',  ( 2.146824126175768122, 20.56989294761467946, 4.842749342374482069 ) ) ;
#5290 = DIRECTION ( 'NONE',  ( 0.000000000000000000, 1.000000000000000000, 0.000000000000000000 ) ) ;
#5291 = CYLINDRICAL_SURFACE ( 'NONE', #9940, 9.524999999999996803 ) ;
#5292 = LINE ( 'NONE', #15502, #13878 ) ;
#5293 = ORIENTED_EDGE ( 'NONE', *, *, #15972, .T. ) ;
#5294 = EDGE_CURVE ( 'NONE', #12469, #4408, #8878, .T. ) ;
#5295 = CARTESIAN_POINT ( 'NONE',  ( 9.692593345077291644, 20.83333359141052199, -1.539594646718391191 ) ) ;
#5296 = ADVANCED_FACE ( 'NONE', ( #2781 ), #13081, .F. ) ;
#5297 = ADVANCED_FACE ( 'NONE', ( #1332 ), #17377, .T. ) ;
#5298 = VECTOR ( 'NONE', #8744, 1000.000000000000000 ) ;
#5299 = DIRECTION ( 'NONE',  ( 0.9579671649362032637, 0.000000000000000000, -0.2868778675745010664 ) ) ;
#5300 = CARTESIAN_POINT ( 'NONE',  ( 13.34857347338189193, 16.50995800865382890, 7.170687989708792287 ) ) ;
#5301 = EDGE_LOOP ( 'NONE', ( #21409, #15071, #12329, #12333, #18326, #2264 ) ) ;
#5302 = EDGE_LOOP ( 'NONE', ( #11580, #11027, #10818, #12451 ) ) ;
#5303 = DIRECTION ( 'NONE',  ( 0.000000000000000000, 1.000000000000000000, 0.000000000000000000 ) ) ;
#5304 = CARTESIAN_POINT ( 'NONE',  ( 9.450549344251921724, 16.49206086971394569, 7.983172913004323412 ) ) ;
#5305 = CARTESIAN_POINT ( 'NONE',  ( 7.265612110562694070, 13.47123956803594069, 6.779132443849506195 ) ) ;
#5306 = CYLINDRICAL_SURFACE ( 'NONE', #20750, 16.66875000000000284 ) ;
#5307 = CARTESIAN_POINT ( 'NONE',  ( 5.812451298883001272, 12.84336716734772210, 0.1757888620865697415 ) ) ;
#5308 = CARTESIAN_POINT ( 'NONE',  ( 7.325623915630060878, 15.12110239233129683, 7.475628130178912478 ) ) ;
#5309 = VECTOR ( 'NONE', #20207, 1000.000000000000000 ) ;
#5310 = CARTESIAN_POINT ( 'NONE',  ( 1.652501564093576292, 20.40137862700089499, 4.418296261410975312 ) ) ;
#5311 = CIRCLE ( 'NONE', #8142, 0.7950200000000000600 ) ;
#5312 = DIRECTION ( 'NONE',  ( 0.000000000000000000, 1.000000000000000000, 0.000000000000000000 ) ) ;
#5313 = CARTESIAN_POINT ( 'NONE',  ( 12.41071875754558640, 10.73085021393864125, 0.5799336287222065511 ) ) ;
#5314 = EDGE_CURVE ( 'NONE', #14268, #20548, #19814, .T. ) ;
#5315 = AXIS2_PLACEMENT_3D ( 'NONE', #9081, #10646, #14091 ) ;
#5316 = CARTESIAN_POINT ( 'NONE',  ( 4.758138823084279601, 20.54266468784728161, 6.821625993668097188 ) ) ;
#5317 = DIRECTION ( 'NONE',  ( 0.8609107660235849613, 0.000000000000000000, -0.5087559856598092844 ) ) ;
#5318 = DIRECTION ( 'NONE',  ( -0.05085730733808142834, 0.000000000000000000, 0.9987059298363657467 ) ) ;
#5319 = CARTESIAN_POINT ( 'NONE',  ( 0.7370043370095074042, 12.12568132066150106, 4.867010393250122746 ) ) ;
#5320 = DIRECTION ( 'NONE',  ( 0.000000000000000000, 1.000000000000000000, 0.000000000000000000 ) ) ;
#5321 = DIRECTION ( 'NONE',  ( 0.000000000000000000, -1.000000000000000000, -0.000000000000000000 ) ) ;
#5322 = CARTESIAN_POINT ( 'NONE',  ( 15.52272087797709332, -8.406786558832781253, -16.18343461258216465 ) ) ;
#5323 = AXIS2_PLACEMENT_3D ( 'NONE', #14791, #21501, #8120 ) ;
#5324 = EDGE_CURVE ( 'NONE', #9688, #15950, #18352, .T. ) ;
#5325 = VECTOR ( 'NONE', #16325, 1000.000000000000114 ) ;
#5326 = CARTESIAN_POINT ( 'NONE',  ( 57.35354854712898742, 2.586003464000000029, -21.22263945788050776 ) ) ;
#5327 = EDGE_CURVE ( 'NONE', #2537, #16536, #10287, .T. ) ;
#5328 = AXIS2_PLACEMENT_3D ( 'NONE', #19831, #19716, #2821 ) ;
#5329 = CARTESIAN_POINT ( 'NONE',  ( 10.47526939876109964, 20.78160439491057332, 5.469098418909443815 ) ) ;
#5330 = ORIENTED_EDGE ( 'NONE', *, *, #14837, .T. ) ;
#5331 = CARTESIAN_POINT ( 'NONE',  ( 11.98942949869243790, 11.25314847078228198, 0.6870342585492783538 ) ) ;
#5332 = CARTESIAN_POINT ( 'NONE',  ( 11.63555623300968556, -3.657949307911554371, -15.72510360806348650 ) ) ;
#5333 = CARTESIAN_POINT ( 'NONE',  ( 21.43124999999999858, 16.27314499999999953, 8.731249999999999289 ) ) ;
#5334 = VERTEX_POINT ( 'NONE', #11506 ) ;
#5335 = PRODUCT_CONTEXT ( 'NONE', #4393, 'mechanical' ) ;
#5336 = CYLINDRICAL_SURFACE ( 'NONE', #4287, 30.16250000000000142 ) ;
#5337 = CARTESIAN_POINT ( 'NONE',  ( 4.623685801006120144, 19.97383893227930329, 1.114202881698282965 ) ) ;
#5338 = DIRECTION ( 'NONE',  ( 0.08420877549337300871, 0.000000000000000000, 0.9964481331860212121 ) ) ;
#5339 = CARTESIAN_POINT ( 'NONE',  ( 6.144469310126137174, 11.61924814016722074, 2.916029993654237984 ) ) ;
#5340 = AXIS2_PLACEMENT_3D ( 'NONE', #8329, #14996, #1684 ) ;
#5341 = VECTOR ( 'NONE', #446, 1000.000000000000114 ) ;
#5342 = VECTOR ( 'NONE', #2094, 1000.000000000000114 ) ;
#5343 = CARTESIAN_POINT ( 'NONE',  ( 10.88152465653400469, -4.868500552888323618, -16.40605285604548413 ) ) ;
#5344 = VERTEX_POINT ( 'NONE', #21344 ) ;
#5345 = CARTESIAN_POINT ( 'NONE',  ( 9.357021909119426439, 17.21976690206051330, -2.890337777318933377 ) ) ;
#5346 = EDGE_CURVE ( 'NONE', #21849, #16032, #9954, .T. ) ;
#5347 = CARTESIAN_POINT ( 'NONE',  ( 6.143851211478567720, 11.87235548079908298, 1.604867153432555593 ) ) ;
#5348 = CARTESIAN_POINT ( 'NONE',  ( 1.061195401963308971, 11.40353646073516103, 4.768344864361504065 ) ) ;
#5349 = EDGE_CURVE ( 'NONE', #6418, #2731, #1230, .T. ) ;
#5350 = CARTESIAN_POINT ( 'NONE',  ( 8.763882600799913547, 20.20007397076694033, 6.602868004581734951 ) ) ;
#5351 = AXIS2_PLACEMENT_3D ( 'NONE', #11406, #7649, #6094 ) ;
#5352 = EDGE_CURVE ( 'NONE', #4463, #5142, #15566, .T. ) ;
#5353 = DIRECTION ( 'NONE',  ( -0.9579671649362033747, 0.000000000000000000, 0.2868778675745011220 ) ) ;
#5354 = CARTESIAN_POINT ( 'NONE',  ( 19.00283808968254107, -0.5370937612277498774, -14.51149966347872677 ) ) ;
#5355 = CARTESIAN_POINT ( 'NONE',  ( -15.39353573898878658, 34.79968030885680008, -10.30107656633069979 ) ) ;
#5356 = ORIENTED_EDGE ( 'NONE', *, *, #18827, .F. ) ;
#5357 = CARTESIAN_POINT ( 'NONE',  ( 13.38426742744203857, 16.76855268369192586, 7.271850668099400394 ) ) ;
#5358 = VECTOR ( 'NONE', #21416, 1000.000000000000000 ) ;
#5359 = ORIENTED_EDGE ( 'NONE', *, *, #11783, .F. ) ;
#5360 = PRESENTATION_LAYER_ASSIGNMENT (  '', '', ( #2139 ) ) ;
#5361 = CARTESIAN_POINT ( 'NONE',  ( 9.360600831854357651, 13.78714971782336107, -2.154141186429150423 ) ) ;
#5362 = PLANE ( 'NONE',  #19736 ) ;
#5363 = CARTESIAN_POINT ( 'NONE',  ( 49.72033008250774344, 42.06303499999999929, -2.687827786179598277 ) ) ;
#5365 = DIRECTION ( 'NONE',  ( -0.3482992169606098365, 0.9330960544336215357, -0.08955115110948595747 ) ) ;
#5364 = CARTESIAN_POINT ( 'NONE',  ( 5.341253238563739458, 21.55539096890324302, 3.869257563646466558 ) ) ;
#5366 = ORIENTED_EDGE ( 'NONE', *, *, #16023, .F. ) ;
#5367 = CARTESIAN_POINT ( 'NONE',  ( 7.432055445221635637, 13.22750976636692677, 7.445346989300424489 ) ) ;
#5368 = VECTOR ( 'NONE', #7621, 1000.000000000000114 ) ;
#5369 = DIRECTION ( 'NONE',  ( 0.000000000000000000, -1.000000000000000000, 0.000000000000000000 ) ) ;
#5370 = ORIENTED_EDGE ( 'NONE', *, *, #8955, .F. ) ;
#5371 = CARTESIAN_POINT ( 'NONE',  ( -23.01875000000000071, 0.000000000000000000, -10.31874999999999964 ) ) ;
#5372 = ORIENTED_EDGE ( 'NONE', *, *, #11517, .F. ) ;
#5373 = AXIS2_PLACEMENT_3D ( 'NONE', #13800, #20736, #10466 ) ;
#5374 = EDGE_CURVE ( 'NONE', #9016, #13089, #12057, .T. ) ;
#5375 = CARTESIAN_POINT ( 'NONE',  ( 42.79471501377724252, 32.54502000000000095, 5.049205022181460834 ) ) ;
#5376 = LINE ( 'NONE', #12139, #3544 ) ;
#5377 = CYLINDRICAL_SURFACE ( 'NONE', #15053, 0.5080000000000000071 ) ;
#5378 = CARTESIAN_POINT ( 'NONE',  ( 3.392010078599061895, 21.32553552010993414, 3.405406787441542349 ) ) ;
#5379 = AXIS2_PLACEMENT_3D ( 'NONE', #3826, #8677, #15451 ) ;
#5380 = CARTESIAN_POINT ( 'NONE',  ( 54.88544852023625253, 38.88803500000000213, -18.42785536490203668 ) ) ;
#5381 = ORIENTED_EDGE ( 'NONE', *, *, #3212, .F. ) ;
#5382 = DIRECTION ( 'NONE',  ( 0.000000000000000000, 0.000000000000000000, 1.000000000000000000 ) ) ;
#5383 = CARTESIAN_POINT ( 'NONE',  ( 46.03750000000000142, -14.84248999999999974, -10.31874999999999964 ) ) ;
#5384 = CARTESIAN_POINT ( 'NONE',  ( 49.79678389823170903, 32.54502000000000095, -28.13445659451038594 ) ) ;
#5386 = CARTESIAN_POINT ( 'NONE',  ( 16.45317959916927109, -7.164694729300216558, -14.76837516743119849 ) ) ;
#5385 = CARTESIAN_POINT ( 'NONE',  ( 44.28293121686854761, -3.968114999999999615, -31.08068102505560759 ) ) ;
#5387 = ORIENTED_EDGE ( 'NONE', *, *, #362, .T. ) ;
#5388 = VERTEX_POINT ( 'NONE', #20423 ) ;
#5389 = CARTESIAN_POINT ( 'NONE',  ( 9.206787867131550840, 14.88153510792360024, 7.130031284213801612 ) ) ;
#5391 = CARTESIAN_POINT ( 'NONE',  ( 14.43917063414567536, 38.48766750000000059, 2.343183994106907697 ) ) ;
#5390 = CARTESIAN_POINT ( 'NONE',  ( 1.754384330265707392, 15.58904521221044170, 9.648152067750672245 ) ) ;
#5392 = ORIENTED_EDGE ( 'NONE', *, *, #9775, .T. ) ;
#5393 = CARTESIAN_POINT ( 'NONE',  ( 5.593119243055995504, 15.65317711712176063, 8.755201639697592242 ) ) ;
#5394 = VECTOR ( 'NONE', #6395, 1000.000000000000114 ) ;
#5395 = EDGE_LOOP ( 'NONE', ( #13484, #6502, #15685, #590 ) ) ;
#5396 = ORIENTED_EDGE ( 'NONE', *, *, #5294, .T. ) ;
#5397 = CARTESIAN_POINT ( 'NONE',  ( 7.484202164504814903, 14.08084388130622244, -1.560156711047595346 ) ) ;
#5398 = VERTEX_POINT ( 'NONE', #5094 ) ;
#5399 = EDGE_CURVE ( 'NONE', #4289, #10917, #21588, .T. ) ;
#5400 = DIRECTION ( 'NONE',  ( 0.08420877549337300871, 0.000000000000000000, 0.9964481331860212121 ) ) ;
#5401 = FACE_OUTER_BOUND ( 'NONE', #8581, .T. ) ;
#5402 = DIRECTION ( 'NONE',  ( 0.000000000000000000, 1.000000000000000000, 0.000000000000000000 ) ) ;
#5403 = CARTESIAN_POINT ( 'NONE',  ( 3.083679442600902654, 19.41275837844778351, 8.177690828459004635 ) ) ;
#5404 = DIRECTION ( 'NONE',  ( 0.9579671649362033747, 0.000000000000000000, -0.2868778675745010664 ) ) ;
#5405 = ORIENTED_EDGE ( 'NONE', *, *, #10056, .F. ) ;
#5406 = CARTESIAN_POINT ( 'NONE',  ( 0.1053325033440700720, 20.71056957386564079, 4.678228806545786433 ) ) ;
#5407 = LINE ( 'NONE', #445, #1815 ) ;
#5408 = CARTESIAN_POINT ( 'NONE',  ( 53.00229660230819917, -5.166360000000002728, -16.81808920586004419 ) ) ;
#5409 = FACE_OUTER_BOUND ( 'NONE', #5851, .T. ) ;
#5410 = ORIENTED_EDGE ( 'NONE', *, *, #19907, .T. ) ;
#5411 = CARTESIAN_POINT ( 'NONE',  ( 8.873261155706039460, 17.35598761042906801, -3.486507808218821225 ) ) ;
#5412 = VECTOR ( 'NONE', #13798, 1000.000000000000000 ) ;
#5413 = DIRECTION ( 'NONE',  ( -0.9685006480810794960, 0.000000000000000000, -0.2490110332224836354 ) ) ;
#5414 = CARTESIAN_POINT ( 'NONE',  ( 13.06466659634344651, 18.75638376262387652, 6.663973104921168122 ) ) ;
#5415 = ORIENTED_EDGE ( 'NONE', *, *, #1285, .T. ) ;
#5416 = ORIENTED_EDGE ( 'NONE', *, *, #8999, .F. ) ;
#5417 = CARTESIAN_POINT ( 'NONE',  ( 47.80475250345343596, 38.88803500000000213, -11.91473563638196786 ) ) ;
#5418 = CARTESIAN_POINT ( 'NONE',  ( 9.004477611269402715, 11.50997377360702245, 5.301999128193525479 ) ) ;
#5419 = CARTESIAN_POINT ( 'NONE',  ( 2.119723087323794442, 17.94179249953145217, 0.2479987765329453031 ) ) ;
#5420 = DIRECTION ( 'NONE',  ( 0.000000000000000000, -1.000000000000000000, -0.000000000000000000 ) ) ;
#5421 = CARTESIAN_POINT ( 'NONE',  ( 5.591081369763479358, 15.58183542640050412, -1.327434291682264345 ) ) ;
#5422 = VECTOR ( 'NONE', #8181, 1000.000000000000000 ) ;
#5423 = DIRECTION ( 'NONE',  ( -0.8193181045417649022, -0.5733392046337750791, 0.000000000000000000 ) ) ;
#5424 = EDGE_CURVE ( 'NONE', #15045, #8192, #20166, .T. ) ;
#5425 = CARTESIAN_POINT ( 'NONE',  ( 7.758187014828991757, 18.34001794662099982, -2.671095701710830550 ) ) ;
#5426 = ADVANCED_FACE ( 'NONE', ( #15396 ), #221, .T. ) ;
#5427 = CARTESIAN_POINT ( 'NONE',  ( 5.031007107017858360, 12.45697886261652698, 5.850013550272263885 ) ) ;
#5428 = CARTESIAN_POINT ( 'NONE',  ( 13.38780373963751202, 21.37707633678951780, 1.836183508607381443 ) ) ;
#5429 = CARTESIAN_POINT ( 'NONE',  ( 1.134588408652542180, 11.63698894629814085, 6.556856509031627311 ) ) ;
#5430 = CARTESIAN_POINT ( 'NONE',  ( 1.031431676875810721, 19.63442241222599094, 8.342029421792293675 ) ) ;
#5431 = CARTESIAN_POINT ( 'NONE',  ( 19.93069405542505379, -0.3168215820087039725, -14.83805648859174653 ) ) ;
#5432 = CARTESIAN_POINT ( 'NONE',  ( -0.6715443117284065622, 20.05178378372840342, 3.977307728984901480 ) ) ;
#5433 = LINE ( 'NONE', #4116, #2837 ) ;
#5434 = CARTESIAN_POINT ( 'NONE',  ( 49.09065990372640442, 30.56064500000000095, -26.70549589918839928 ) ) ;
#5435 = CARTESIAN_POINT ( 'NONE',  ( 17.33536478547116033, -8.249904329601282171, -15.78574727907301067 ) ) ;
#5436 = CIRCLE ( 'NONE', #12536, 16.66874999999998508 ) ;
#5437 = CARTESIAN_POINT ( 'NONE',  ( 14.43917063414567536, -6.754812500000002551, 2.343183994106907697 ) ) ;
#5438 = CARTESIAN_POINT ( 'NONE',  ( 61.02111788801703085, 0.000000000000000000, -5.406220493519755088 ) ) ;
#5439 = CARTESIAN_POINT ( 'NONE',  ( 11.01646722322404948, 19.16985564352501825, 6.846897438552763226 ) ) ;
#5440 = DIRECTION ( 'NONE',  ( -0.8741107132214044340, 0.000000000000000000, -0.4857267349359799535 ) ) ;
#5441 = CARTESIAN_POINT ( 'NONE',  ( 11.94991743495628356, 11.28343550310636090, 0.5166888111268383987 ) ) ;
#5442 = CARTESIAN_POINT ( 'NONE',  ( 7.735533989518945219, 25.39269750000000059, -21.17236077523805449 ) ) ;
#5443 = CARTESIAN_POINT ( 'NONE',  ( 0.6077902027026849119, 19.54577606275120161, 7.429059100087549439 ) ) ;
#5444 = VECTOR ( 'NONE', #6440, 1000.000000000000000 ) ;
#5445 = ORIENTED_EDGE ( 'NONE', *, *, #12917, .F. ) ;
#5446 = APPLICATION_PROTOCOL_DEFINITION ( 'draft international standard', 'automotive_design', 1998, #18349 ) ;
#5447 = EDGE_CURVE ( 'NONE', #11597, #3189, #3434, .T. ) ;
#5448 = CARTESIAN_POINT ( 'NONE',  ( 1.532169971477637782, -1.500984687155947128, -20.71839214105750315 ) ) ;
#5449 = CARTESIAN_POINT ( 'NONE',  ( 26.59062499999999929, 1.984375000000000000, -2.268784209304649746 ) ) ;
#5450 = FACE_OUTER_BOUND ( 'NONE', #4875, .T. ) ;
#5451 = CIRCLE ( 'NONE', #17839, 0.3962400000000008138 ) ;
#5452 = ORIENTED_EDGE ( 'NONE', *, *, #20067, .F. ) ;
#5453 = CARTESIAN_POINT ( 'NONE',  ( 6.570365227786298057, 11.61181900198992167, 3.191872150317673018 ) ) ;
#5454 = EDGE_CURVE ( 'NONE', #7062, #21627, #2090, .T. ) ;
#5455 = CARTESIAN_POINT ( 'NONE',  ( 8.041622239940769745, 19.55876953989094247, -1.099914718329432439 ) ) ;
#5456 = CARTESIAN_POINT ( 'NONE',  ( 0.1525355661814789543, 13.94977879502390294, 0.5504633849951708902 ) ) ;
#5457 = DIRECTION ( 'NONE',  ( 0.9784543669157947932, 0.000000000000000000, 0.2064631973582977953 ) ) ;
#5458 = LINE ( 'NONE', #18941, #14299 ) ;
#5459 = CARTESIAN_POINT ( 'NONE',  ( 16.90052181627606132, 0.9448800882039219973, -15.17889571493881107 ) ) ;
#5460 = UNCERTAINTY_MEASURE_WITH_UNIT (LENGTH_MEASURE( 1.000000000000000082E-05 ), #19516, 'distance_accuracy_value', 'NONE');
#5461 = CARTESIAN_POINT ( 'NONE',  ( -13.49374999999999858, 1.984375000000000000, 0.000000000000000000 ) ) ;
#5462 = ORIENTED_EDGE ( 'NONE', *, *, #11884, .F. ) ;
#5463 = CARTESIAN_POINT ( 'NONE',  ( 13.43775099319997146, 14.65538885420913573, 7.055912018318879042 ) ) ;
#5464 = CIRCLE ( 'NONE', #12564, 3.970019999999997662 ) ;
#5465 = ORIENTED_EDGE ( 'NONE', *, *, #4422, .T. ) ;
#5466 = CARTESIAN_POINT ( 'NONE',  ( 10.00073136103841343, 11.49997002360925080, 0.8636844994430420419 ) ) ;
#5467 = DIRECTION ( 'NONE',  ( 0.9685006480810792739, 0.000000000000000000, 0.2490110332224850509 ) ) ;
#5468 = CARTESIAN_POINT ( 'NONE',  ( 13.39756118469465029, 22.16307784260286340, 1.948616576935187750 ) ) ;
#5470 = DIRECTION ( 'NONE',  ( -0.8609107660235850723, 0.000000000000000000, 0.5087559856598092844 ) ) ;
#5469 = CARTESIAN_POINT ( 'NONE',  ( 3.224325801286248794, 13.16763011922862070, 8.241763163179413709 ) ) ;
#5471 = EDGE_LOOP ( 'NONE', ( #14394, #14567 ) ) ;
#5472 = CARTESIAN_POINT ( 'NONE',  ( 6.495082362213654648, 10.90869521295860167, 3.280822230635792369 ) ) ;
#5473 = EDGE_CURVE ( 'NONE', #18633, #6373, #15501, .T. ) ;
#5474 = ADVANCED_FACE ( 'NONE', ( #7073 ), #5291, .F. ) ;
#5475 = CARTESIAN_POINT ( 'NONE',  ( 17.02725982432203367, 34.52875999999999834, -14.27444360421403857 ) ) ;
#5476 = EDGE_LOOP ( 'NONE', ( #11894, #17910 ) ) ;
#5477 = DIRECTION ( 'NONE',  ( 0.000000000000000000, 1.000000000000000000, -1.313388458492437221E-14 ) ) ;
#5478 = CARTESIAN_POINT ( 'NONE',  ( 0.07294454634050162589, 16.38620845716783592, 0.7942576904715414887 ) ) ;
#5479 = DIRECTION ( 'NONE',  ( -0.9964481331860212121, 0.000000000000000000, 0.08420877549337336954 ) ) ;
#5480 = EDGE_LOOP ( 'NONE', ( #16344, #516, #19004, #13353 ) ) ;
#5481 = DIRECTION ( 'NONE',  ( 0.000000000000000000, 1.000000000000000000, 0.000000000000000000 ) ) ;
#5482 = CARTESIAN_POINT ( 'NONE',  ( 1.965037718003479705, 16.82931600788473503, 0.08433362572124197820 ) ) ;
#5483 = AXIS2_PLACEMENT_3D ( 'NONE', #10192, #3568, #20451 ) ;
#5484 = LINE ( 'NONE', #14031, #7503 ) ;
#5485 = LINE ( 'NONE', #7161, #7416 ) ;
#5486 = CARTESIAN_POINT ( 'NONE',  ( 53.92979111630407374, -6.356984999999459873, -15.65141968182990162 ) ) ;
#5487 = DIRECTION ( 'NONE',  ( -0.6702301885068639997, 0.000000000000000000, -0.7421532822901570903 ) ) ;
#5488 = ORIENTED_EDGE ( 'NONE', *, *, #6705, .T. ) ;
#5489 = DIRECTION ( 'NONE',  ( 0.2490110332224850231, 0.000000000000000000, -0.9685006480810791629 ) ) ;
#5490 = CARTESIAN_POINT ( 'NONE',  ( 7.241402720468077092, 24.59767750000000319, -19.25049230170216319 ) ) ;
#5492 = CARTESIAN_POINT ( 'NONE',  ( 19.80715417040793369, -3.131469232938576042, -14.17398794668478601 ) ) ;
#5491 = CARTESIAN_POINT ( 'NONE',  ( -17.46249999999999858, 0.000000000000000000, 0.000000000000000000 ) ) ;
#5493 = EDGE_LOOP ( 'NONE', ( #20747, #8034, #13696, #5588, #16901, #5041, #17997, #21400, #15815, #14066, #20542, #12274, #8699, #1757, #16589, #5238, #18655, #6845, #12571, #11448, #19044, #11895, #12905, #3342 ) ) ;
#5494 = ORIENTED_EDGE ( 'NONE', *, *, #8493, .T. ) ;
#5495 = CARTESIAN_POINT ( 'NONE',  ( 12.71261977860552861, 11.95028677413862184, 4.239190098976814980 ) ) ;
#5497 = CARTESIAN_POINT ( 'NONE',  ( 44.28293121686854761, 36.51313500000000545, -31.08068102505560759 ) ) ;
#5496 = CARTESIAN_POINT ( 'NONE',  ( 2.500687340046055418, 20.82590581279646003, 6.616773250763320569 ) ) ;
#5498 = ORIENTED_EDGE ( 'NONE', *, *, #3446, .F. ) ;
#5500 = CARTESIAN_POINT ( 'NONE',  ( 10.39684359234162692, -3.119971281104964689, -17.24762880647101682 ) ) ;
#5499 = CARTESIAN_POINT ( 'NONE',  ( 4.167336224285882018, 11.37672557165839216, 2.018609927143729887 ) ) ;
#5501 = EDGE_LOOP ( 'NONE', ( #12356, #8368, #21108, #2840 ) ) ;
#5502 = EDGE_CURVE ( 'NONE', #7588, #17030, #2899, .T. ) ;
#5503 = VERTEX_POINT ( 'NONE', #20545 ) ;
#5504 =( REPRESENTATION_RELATIONSHIP ('NONE','NONE', #15554, #3526 ) REPRESENTATION_RELATIONSHIP_WITH_TRANSFORMATION ( #486 )SHAPE_REPRESENTATION_RELATIONSHIP( ) );
#5505 = CARTESIAN_POINT ( 'NONE',  ( 7.926815946483072750, 11.95748302575823097, 0.6454573217223682491 ) ) ;
#5506 = ORIENTED_EDGE ( 'NONE', *, *, #12874, .F. ) ;
#5507 = CARTESIAN_POINT ( 'NONE',  ( 3.415768019861648241, 14.56304571309649099, 8.070112825631751363 ) ) ;
#5508 = DIRECTION ( 'NONE',  ( 0.2490110332224850509, 0.000000000000000000, -0.9685006480810792739 ) ) ;
#5509 = CARTESIAN_POINT ( 'NONE',  ( 13.67756757867809725, -5.959792500000001603, 2.571257636385987144 ) ) ;
#5510 = CARTESIAN_POINT ( 'NONE',  ( 38.23013820809905638, -1.983739999999999837, -14.22485453658974031 ) ) ;
#5511 = DIRECTION ( 'NONE',  ( -0.2868778675745010664, 0.000000000000000000, -0.9579671649362032637 ) ) ;
#5512 = CARTESIAN_POINT ( 'NONE',  ( 13.86631606410951534, 16.88209101360638797, -18.21726315170741017 ) ) ;
#5513 = CARTESIAN_POINT ( 'NONE',  ( 3.401254764629610960, 18.09646818108351951, 8.897540692196587386 ) ) ;
#5514 = LINE ( 'NONE', #7295, #11579 ) ;
#5515 = ORIENTED_EDGE ( 'NONE', *, *, #16413, .F. ) ;
#5516 = CARTESIAN_POINT ( 'NONE',  ( 2.278141381403417931, 20.88642215721691997, 4.832218429395563675 ) ) ;
#5517 = CARTESIAN_POINT ( 'NONE',  ( 9.335363283976800375, -3.968114999999999615, -14.20581391854862474 ) ) ;
#5518 = CARTESIAN_POINT ( 'NONE',  ( 11.82678039945931481, 34.52875999999999834, -12.74436900065013667 ) ) ;
#5519 = ORIENTED_EDGE ( 'NONE', *, *, #3459, .F. ) ;
#5520 = ORIENTED_EDGE ( 'NONE', *, *, #21503, .F. ) ;
#5521 = CARTESIAN_POINT ( 'NONE',  ( 5.089424605553659831, 13.78737461787913077, -1.074966794023267003 ) ) ;
#5522 = AXIS2_PLACEMENT_3D ( 'NONE', #11539, #21598, #3137 ) ;
#5523 = CARTESIAN_POINT ( 'NONE',  ( 3.360635606688116894, -14.84248999999999974, -20.45316710734507026 ) ) ;
#5524 = CARTESIAN_POINT ( 'NONE',  ( 13.22906167343631090, 12.77717586684420148, 6.020701791080536047 ) ) ;
#5525 = EDGE_LOOP ( 'NONE', ( #1871, #15386, #17941, #3065 ) ) ;
#5526 = ORIENTED_EDGE ( 'NONE', *, *, #8979, .T. ) ;
#5527 = EDGE_CURVE ( 'NONE', #11596, #14232, #13960, .T. ) ;
#5528 = CARTESIAN_POINT ( 'NONE',  ( 13.28298931428452967, 21.40937655264818318, 1.617576389153118743 ) ) ;
#5529 = CARTESIAN_POINT ( 'NONE',  ( 8.692839774141368991, 10.93259986899979097, 3.963448146918763904 ) ) ;
#5530 = CARTESIAN_POINT ( 'NONE',  ( 1.098079023573843571, 12.39565097329668042, 6.272954462318547364 ) ) ;
#5531 = CARTESIAN_POINT ( 'NONE',  ( 32.42378190387104553, 34.52875999999999834, -18.15178106273469183 ) ) ;
#5532 = CARTESIAN_POINT ( 'NONE',  ( 5.598276747425085631, 15.82787884806641188, -1.362751658015930012 ) ) ;
#5533 = CARTESIAN_POINT ( 'NONE',  ( 46.03750000000000142, -1.983739999999999393, -10.31874999999999964 ) ) ;
#5534 = FACE_OUTER_BOUND ( 'NONE', #13354, .T. ) ;
#5535 = VECTOR ( 'NONE', #12022, 1000.000000000000000 ) ;
#5536 = CARTESIAN_POINT ( 'NONE',  ( 8.500561619910278921, 21.25109391276654236, 4.936867450891936571 ) ) ;
#5537 = CARTESIAN_POINT ( 'NONE',  ( 21.25660046192028929, -1.983739999999999393, -13.18703856829094079 ) ) ;
#5538 = CARTESIAN_POINT ( 'NONE',  ( 3.536356009984624293, 13.65508413018860168, -0.8098419684375965932 ) ) ;
#5539 = DIRECTION ( 'NONE',  ( 0.9579671649362032637, 0.000000000000000000, -0.2868778675745010664 ) ) ;
#5540 = CARTESIAN_POINT ( 'NONE',  ( 20.23338050908548880, -1.212044145622726443, -14.75678302155165511 ) ) ;
#5541 = CARTESIAN_POINT ( 'NONE',  ( 2.180285587184756402, 12.53249658949568257, 2.158027021525236400 ) ) ;
#5542 = DIRECTION ( 'NONE',  ( 1.000000000000000000, 0.000000000000000000, 0.000000000000000000 ) ) ;
#5543 = FACE_OUTER_BOUND ( 'NONE', #9438, .T. ) ;
#5544 = CARTESIAN_POINT ( 'NONE',  ( 16.36168651129493412, 2.265146188987181120, -15.35027226876440842 ) ) ;
#5545 = CYLINDRICAL_SURFACE ( 'NONE', #2879, 0.5080000000000022276 ) ;
#5546 = DIRECTION ( 'NONE',  ( 0.2868778675745010664, 0.000000000000000000, 0.9579671649362032637 ) ) ;
#5547 = CARTESIAN_POINT ( 'NONE',  ( 9.783420551838821311, 21.71607306610668076, 3.592949344949918355 ) ) ;
#5548 = ORIENTED_EDGE ( 'NONE', *, *, #10174, .F. ) ;
#5549 = CARTESIAN_POINT ( 'NONE',  ( 61.83151161312219557, 32.54502000000000095, -0.3645647634491749334 ) ) ;
#5550 = EDGE_CURVE ( 'NONE', #13568, #16035, #3962, .T. ) ;
#5551 = CARTESIAN_POINT ( 'NONE',  ( 11.84502782025289847, 11.38735974601924283, 0.06333640615650359962 ) ) ;
#5552 = VECTOR ( 'NONE', #20853, 1000.000000000000000 ) ;
#5553 = CARTESIAN_POINT ( 'NONE',  ( 20.36530192851249410, -3.329039984996891910, -15.30396146910969968 ) ) ;
#5554 = CARTESIAN_POINT ( 'NONE',  ( 0.7231469830875896232, 19.66626656054290123, 2.290770552806581595 ) ) ;
#5555 = ORIENTED_EDGE ( 'NONE', *, *, #17087, .T. ) ;
#5556 = LINE ( 'NONE', #7443, #19089 ) ;
#5557 = CARTESIAN_POINT ( 'NONE',  ( 4.471143474535477225, 19.65688249982645175, 0.7326053640163348035 ) ) ;
#5558 = CARTESIAN_POINT ( 'NONE',  ( -29.36874999999999858, 30.56064500000000095, 8.335010000000000474 ) ) ;
#5559 = CARTESIAN_POINT ( 'NONE',  ( 10.51408890650479755, -3.826186581119058072, -16.12191821389345492 ) ) ;
#5560 = VERTEX_POINT ( 'NONE', #15167 ) ;
#5561 = CARTESIAN_POINT ( 'NONE',  ( 9.102730975966599303, 18.23105645554593934, 6.913738234213362865 ) ) ;
#5562 = CARTESIAN_POINT ( 'NONE',  ( 4.789876627565358369, 19.17887308449560635, 7.014825586549866543 ) ) ;
#5563 = FACE_OUTER_BOUND ( 'NONE', #120, .T. ) ;
#5564 = CARTESIAN_POINT ( 'NONE',  ( 7.828653474077823304, 16.61588919119046182, 7.980077449799868106 ) ) ;
#5565 = CARTESIAN_POINT ( 'NONE',  ( 11.52440248773281617, 20.24847620595872044, -3.116674102378380162 ) ) ;
#5566 = AXIS2_PLACEMENT_3D ( 'NONE', #5089, #8720, #5404 ) ;
#5567 = DIRECTION ( 'NONE',  ( -0.4987171968201988270, 0.000000000000000000, 0.8667647648559574369 ) ) ;
#5568 = EDGE_CURVE ( 'NONE', #11596, #7807, #3878, .T. ) ;
#5569 = DIRECTION ( 'NONE',  ( -0.3482992169606098365, 0.9330960544336215357, -0.08955115110948595747 ) ) ;
#5570 = ORIENTED_EDGE ( 'NONE', *, *, #9400, .T. ) ;
#5571 = CARTESIAN_POINT ( 'NONE',  ( 5.350757514931804515, 15.44490212850582189, -2.194769716375351898 ) ) ;
#5572 = DIRECTION ( 'NONE',  ( -0.6496772031432439531, 0.000000000000000000, 0.7602101891687401691 ) ) ;
#5573 = ORIENTED_EDGE ( 'NONE', *, *, #454, .F. ) ;
#5574 = EDGE_CURVE ( 'NONE', #14379, #4173, #17393, .T. ) ;
#5575 = CARTESIAN_POINT ( 'NONE',  ( 9.375099485748442874, 13.64553664392443011, -2.068740140728067889 ) ) ;
#5576 = DIRECTION ( 'NONE',  ( -0.6702301885068628895, 0.000000000000000000, -0.7421532822901579785 ) ) ;
#5577 = CARTESIAN_POINT ( 'NONE',  ( 11.75439013559175017, -1.983739999999999393, 4.331204221326972359 ) ) ;
#5578 = EDGE_CURVE ( 'NONE', #3364, #8815, #552, .T. ) ;
#5580 = DIRECTION ( 'NONE',  ( -0.6702301885068632226, 0.000000000000000000, -0.7421532822901577564 ) ) ;
#5579 = CARTESIAN_POINT ( 'NONE',  ( -0.1742194648750999830, 20.56733048332889879, 6.416404061768046674 ) ) ;
#5581 = ORIENTED_EDGE ( 'NONE', *, *, #14126, .T. ) ;
#5582 = CARTESIAN_POINT ( 'NONE',  ( 7.219865183778306772, 12.09587256105000641, 6.418183704565048942 ) ) ;
#5583 = DIRECTION ( 'NONE',  ( 0.000000000000000000, 1.000000000000000000, 0.000000000000000000 ) ) ;
#5584 = CIRCLE ( 'NONE', #13372, 0.7950200000000012812 ) ;
#5585 = EDGE_LOOP ( 'NONE', ( #12224, #2485, #18899, #3580 ) ) ;
#5586 = LINE ( 'NONE', #12345, #17086 ) ;
#5587 = CARTESIAN_POINT ( 'NONE',  ( 11.60094225694622772, -3.109384115592202402, -16.85129956413878816 ) ) ;
#5588 = ORIENTED_EDGE ( 'NONE', *, *, #4538, .T. ) ;
#5589 = DIRECTION ( 'NONE',  ( -0.08420877549337300871, 0.000000000000000000, -0.9964481331860212121 ) ) ;
#5590 = CARTESIAN_POINT ( 'NONE',  ( 2.014813869672630098, 17.23626398232610057, 0.1440630847629725264 ) ) ;
#5591 = CARTESIAN_POINT ( 'NONE',  ( 9.222712265903270534, 13.32230603934784163, -2.943534436737037741 ) ) ;
#5592 = LINE ( 'NONE', #5716, #11038 ) ;
#5593 = EDGE_CURVE ( 'NONE', #9048, #16262, #2653, .T. ) ;
#5594 = DIRECTION ( 'NONE',  ( -0.7421532822901572013, 0.000000000000000000, 0.6702301885068637777 ) ) ;
#5595 = CARTESIAN_POINT ( 'NONE',  ( -17.46249999999999858, -0.3962399999999990929, 0.000000000000000000 ) ) ;
#5596 = PRODUCT_DEFINITION ( 'UNKNOWN', '', #10181, #20483 ) ;
#5597 = CIRCLE ( 'NONE', #6655, 1.191259999999999319 ) ;
#5598 = VERTEX_POINT ( 'NONE', #15828 ) ;
#5599 = DIRECTION ( 'NONE',  ( -0.9784543669157947932, 0.000000000000000000, -0.2064631973582977953 ) ) ;
#5600 = DIRECTION ( 'NONE',  ( -0.9964481331860213231, 0.000000000000000000, 0.08420877549337293932 ) ) ;
#5601 = CARTESIAN_POINT ( 'NONE',  ( -12.30312499999999964, 1.984375000000000000, 8.335010000000000474 ) ) ;
#5603 = CARTESIAN_POINT ( 'NONE',  ( -12.30312499999999964, 1.984375000000000000, 8.335010000000000474 ) ) ;
#5602 = PLANE ( 'NONE',  #15892 ) ;
#5604 = ORIENTED_EDGE ( 'NONE', *, *, #16092, .F. ) ;
#5605 = ORIENTED_EDGE ( 'NONE', *, *, #8285, .F. ) ;
#5606 = CARTESIAN_POINT ( 'NONE',  ( 5.828080763218296489, 12.69966494906990206, 0.1882201014488152913 ) ) ;
#5608 = FACE_OUTER_BOUND ( 'NONE', #16059, .T. ) ;
#5607 = CARTESIAN_POINT ( 'NONE',  ( 0.7899212862509950028, 11.31684784372412089, 4.849392175464794619 ) ) ;
#5609 = VERTEX_POINT ( 'NONE', #14382 ) ;
#5611 = CARTESIAN_POINT ( 'NONE',  ( 20.79919319928621846, -3.365577675197465535, -14.45920257639869355 ) ) ;
#5610 = CARTESIAN_POINT ( 'NONE',  ( 5.537923952358154267, 16.68662888302730707, 8.792294931775872513 ) ) ;
#5612 = AXIS2_PLACEMENT_3D ( 'NONE', #21252, #5672, #19371 ) ;
#5613 = EDGE_LOOP ( 'NONE', ( #15507, #18949, #21847, #11900 ) ) ;
#5614 = ORIENTED_EDGE ( 'NONE', *, *, #4909, .F. ) ;
#5615 = CARTESIAN_POINT ( 'NONE',  ( 7.439309206678073494, 15.11921583032367877, -1.967807152704160734 ) ) ;
#5616 = CARTESIAN_POINT ( 'NONE',  ( 1.422955370182567014, 13.97322825811035685, 8.124243789848305752 ) ) ;
#5617 = VECTOR ( 'NONE', #2061, 1000.000000000000114 ) ;
#5618 = ORIENTED_EDGE ( 'NONE', *, *, #19742, .T. ) ;
#5619 = AXIS2_PLACEMENT_3D ( 'NONE', #16345, #7602, #7812 ) ;
#5620 = DIRECTION ( 'NONE',  ( 0.08420877549337302259, 0.000000000000000000, 0.9964481331860212121 ) ) ;
#5621 = EDGE_CURVE ( 'NONE', #1096, #17189, #21001, .T. ) ;
#5622 = CIRCLE ( 'NONE', #10572, 19.05000000000000071 ) ;
#5623 = CYLINDRICAL_SURFACE ( 'NONE', #2968, 0.7950200000000003930 ) ;
#5624 = CARTESIAN_POINT ( 'NONE',  ( 5.430521817098937554, 34.12394749999999988, -21.76500205408690647 ) ) ;
#5625 = CARTESIAN_POINT ( 'NONE',  ( 1.715417743616410196, 21.19999865368947312, 4.581887404234925576 ) ) ;
#5626 = EDGE_CURVE ( 'NONE', #6593, #14525, #7299, .T. ) ;
#5627 = CARTESIAN_POINT ( 'NONE',  ( 19.75611402437074560, -4.719049260853012129, -15.34047214062004372 ) ) ;
#5628 = VERTEX_POINT ( 'NONE', #9382 ) ;
#5629 = CARTESIAN_POINT ( 'NONE',  ( 6.980491476190183064, 11.62550227300026151, 4.018716726805900308 ) ) ;
#5630 = LINE ( 'NONE', #12056, #7479 ) ;
#5631 = CARTESIAN_POINT ( 'NONE',  ( 59.52193197173441774, 32.54502000000000095, -3.260183413611184911 ) ) ;
#5632 = CARTESIAN_POINT ( 'NONE',  ( 61.04701390398659555, 34.52875999999999834, -15.15157976445104993 ) ) ;
#5633 = CARTESIAN_POINT ( 'NONE',  ( 32.17043356788648367, 2.586003464000000029, -17.71146456218788146 ) ) ;
#5634 = ORIENTED_EDGE ( 'NONE', *, *, #16460, .F. ) ;
#5635 = ORIENTED_EDGE ( 'NONE', *, *, #2543, .F. ) ;
#5636 = CARTESIAN_POINT ( 'NONE',  ( 9.445988718791797467, 11.13211821786026157, 0.4531721362220474947 ) ) ;
#5637 = FACE_OUTER_BOUND ( 'NONE', #12030, .T. ) ;
#5638 = CARTESIAN_POINT ( 'NONE',  ( 13.25983584171517116, 12.99030557094804550, 6.173116066625142118 ) ) ;
#5639 = VERTEX_POINT ( 'NONE', #19117 ) ;
#5640 = PRODUCT_DEFINITION_SHAPE ( 'NONE', 'NONE',  #21888 ) ;
#5641 = EDGE_LOOP ( 'NONE', ( #20856, #6335, #176, #12785 ) ) ;
#5642 = LINE ( 'NONE', #3664, #10236 ) ;
#5643 = CARTESIAN_POINT ( 'NONE',  ( 7.655173456064148674, 19.24630943483592205, -2.133094473368749355 ) ) ;
#5644 = CARTESIAN_POINT ( 'NONE',  ( 6.336034323945050062, 11.65589518700730132, 2.459063698344419180 ) ) ;
#5645 = CARTESIAN_POINT ( 'NONE',  ( 28.97711086133420366, 32.54502000000000095, -10.31874999999999964 ) ) ;
#5646 = CIRCLE ( 'NONE', #20449, 0.5080000000000006732 ) ;
#5647 = CIRCLE ( 'NONE', #7044, 0.7950200000000000600 ) ;
#5648 = CARTESIAN_POINT ( 'NONE',  ( 6.077993251687278331, 12.04737542433794495, 1.424762966830985356 ) ) ;
#5649 = CARTESIAN_POINT ( 'NONE',  ( 7.225041933885432144, 13.52979383919193701, 6.708482075865046745 ) ) ;
#5650 = LINE ( 'NONE', #10747, #7881 ) ;
#5651 = DIRECTION ( 'NONE',  ( -0.000000000000000000, -1.000000000000000000, 0.000000000000000000 ) ) ;
#5652 = AXIS2_PLACEMENT_3D ( 'NONE', #1773, #1456, #9968 ) ;
#5653 = CARTESIAN_POINT ( 'NONE',  ( 10.60828838171844524, 10.54134736952624252, 2.111780394654666715 ) ) ;
#5654 = CARTESIAN_POINT ( 'NONE',  ( 2.262747632565262013, 19.81152135836902062, 0.4607135673276451238 ) ) ;
#5655 = CARTESIAN_POINT ( 'NONE',  ( 0.1974682674717982978, 20.91554504214090926, 6.174409461716068748 ) ) ;
#5656 = ADVANCED_FACE ( 'NONE', ( #21097 ), #14063, .T. ) ;
#5657 = CYLINDRICAL_SURFACE ( 'NONE', #6459, 9.524999999999996803 ) ;
#5658 = CIRCLE ( 'NONE', #20471, 1.984374999999998890 ) ;
#5659 = CARTESIAN_POINT ( 'NONE',  ( 4.210766624584501017, 12.02909395710813989, 2.263615127930675541 ) ) ;
#5660 = DIRECTION ( 'NONE',  ( -0.2868778675745011220, 0.000000000000000000, -0.9579671649362033747 ) ) ;
#5661 = CYLINDRICAL_SURFACE ( 'NONE', #8526, 0.5953124999999994671 ) ;
#5662 = CARTESIAN_POINT ( 'NONE',  ( 17.19104467599775532, 2.097219702267779429, -15.10484033739021648 ) ) ;
#5663 = CIRCLE ( 'NONE', #17312, 0.5079999999999973426 ) ;
#5664 = CARTESIAN_POINT ( 'NONE',  ( 0.7843704457339527591, 5.548947500000001476, -23.55949434567611078 ) ) ;
#5665 = DIRECTION ( 'NONE',  ( 0.000000000000000000, 1.000000000000000000, 0.000000000000000000 ) ) ;
#5666 = CARTESIAN_POINT ( 'NONE',  ( 10.89352820671717836, 11.26631715233412301, 4.659004019323803369 ) ) ;
#5667 = VERTEX_POINT ( 'NONE', #12605 ) ;
#5668 = LINE ( 'NONE', #3797, #2529 ) ;
#5669 = CARTESIAN_POINT ( 'NONE',  ( 11.30708403999637923, 13.02122886099977173, -2.389217618889588390 ) ) ;
#5670 = AXIS2_PLACEMENT_3D ( 'NONE', #5703, #12572, #14243 ) ;
#5671 = CARTESIAN_POINT ( 'NONE',  ( 5.999549737364129776, 11.29786724840421108, 1.172376165605415910 ) ) ;
#5672 = DIRECTION ( 'NONE',  ( -0.9987059298363656357, 0.000000000000000000, -0.05085730733808393328 ) ) ;
#5673 = CARTESIAN_POINT ( 'NONE',  ( -0.05205347293826909777, 14.29405283160754614, 1.280296971734305567 ) ) ;
#5674 = VERTEX_POINT ( 'NONE', #9157 ) ;
#5675 = DIRECTION ( 'NONE',  ( 0.2490110332224846623, 0.000000000000000000, -0.9685006480810793850 ) ) ;
#5676 = AXIS2_PLACEMENT_3D ( 'NONE', #21844, #13355, #1614 ) ;
#5677 = CARTESIAN_POINT ( 'NONE',  ( 52.69799253609296130, -5.166360000000003616, -16.33142188479335744 ) ) ;
#5678 = ORIENTED_EDGE ( 'NONE', *, *, #1777, .T. ) ;
#5679 = CARTESIAN_POINT ( 'NONE',  ( 13.28541201854497089, 14.87610706663238247, 6.283089683201566800 ) ) ;
#5680 = VECTOR ( 'NONE', #14902, 1000.000000000000000 ) ;
#5681 = CARTESIAN_POINT ( 'NONE',  ( 13.10321590180860163, 13.21942167511952171, 5.511931958094891115 ) ) ;
#5682 = CARTESIAN_POINT ( 'NONE',  ( 12.11531023645522431, 21.60439101236092085, -1.537999855465251198 ) ) ;
#5683 = ADVANCED_FACE ( 'NONE', ( #11051 ), #19439, .F. ) ;
#5684 = CIRCLE ( 'NONE', #6735, 3.175000000000000711 ) ;
#5685 = AXIS2_PLACEMENT_3D ( 'NONE', #3608, #280, #3394 ) ;
#5686 = CARTESIAN_POINT ( 'NONE',  ( 20.23508918937977796, -1.359453322992689506, -14.75410208910826704 ) ) ;
#5687 = CARTESIAN_POINT ( 'NONE',  ( 13.72785506320953353, 0.4691747601981155480, -16.15643954551278938 ) ) ;
#5688 = UNCERTAINTY_MEASURE_WITH_UNIT (LENGTH_MEASURE( 1.000000000000000082E-05 ), #16367, 'distance_accuracy_value', 'NONE');
#5689 = LINE ( 'NONE', #12560, #6385 ) ;
#5690 = VERTEX_POINT ( 'NONE', #5631 ) ;
#5691 = CARTESIAN_POINT ( 'NONE',  ( 7.402035373046037314, 12.62799681450196054, -1.657535778544305671 ) ) ;
#5692 = CARTESIAN_POINT ( 'NONE',  ( 21.29044094599970904, -2.646515516688929814, -13.86205913043574434 ) ) ;
#5693 = CIRCLE ( 'NONE', #3219, 30.16249999999998721 ) ;
#5694 = CARTESIAN_POINT ( 'NONE',  ( 52.43047507149418607, 39.68795354937129360, -17.37982868320523977 ) ) ;
#5695 = ORIENTED_EDGE ( 'NONE', *, *, #4747, .T. ) ;
#5696 = CARTESIAN_POINT ( 'NONE',  ( 9.348107690663828961, 13.91467961181269786, -2.228914411464946177 ) ) ;
#5697 = PLANE ( 'NONE',  #372 ) ;
#5698 = CARTESIAN_POINT ( 'NONE',  ( 13.03561731774868093, 22.21723951419428289, 0.9385846051497386267 ) ) ;
#5700 = FACE_OUTER_BOUND ( 'NONE', #14500, .T. ) ;
#5699 = CARTESIAN_POINT ( 'NONE',  ( 3.293281583389384704, 17.27089909971514103, -0.9423259528885826741 ) ) ;
#5701 = ORIENTED_EDGE ( 'NONE', *, *, #5346, .T. ) ;
#5702 = CARTESIAN_POINT ( 'NONE',  ( 7.543722629209693942, 14.82614142317876116, 8.183702551990444718 ) ) ;
#5703 = CARTESIAN_POINT ( 'NONE',  ( -29.36874999999999858, 1.983739999999999837, 8.731885000000000119 ) ) ;
#5704 = CLOSED_SHELL ( 'NONE', ( #5174, #19745, #3025, #8258, #14701, #18661, #9504, #823, #12021, #11364, #8124, #11300, #10854, #10855, #14142, #12280, #17188, #9327, #12372, #20334, #1779, #2103, #16522, #7803, #20562, #17570, #13980, #5296, #3968, #3277, #10029, #18041, #899, #15115, #13762, #19133, #4019, #18292, #556, #12076, #6490, #4664, #5028, #12566, #4821, #12235, #11974, #211, #9747, #8298, #16237, #16302, #3745, #8203, #6531, #19926, #13876, #2160, #13715, #20591, #7500, #4865, #11397, #13095, #20936, #5474, #10331, #898, #3698, #10903, #1517, #519, #18676, #12629, #15157, #1431, #10175, #16801, #16824, #10779, #21397, #8714, #15213, #9942, #17520, #15183, #451, #11575, #2886, #11554, #4884, #88, #618, #2473, #15888, #1377 ) ) ;
#5705 = CARTESIAN_POINT ( 'NONE',  ( 42.79471501377724252, -1.983739999999999837, 5.049205022181460834 ) ) ;
#5706 = ORIENTED_EDGE ( 'NONE', *, *, #4378, .F. ) ;
#5707 = CARTESIAN_POINT ( 'NONE',  ( 19.38236331922507816, 0.4371055082821885263, -15.00287587734002059 ) ) ;
#5708 = EDGE_CURVE ( 'NONE', #13402, #15989, #14529, .T. ) ;
#5709 = VECTOR ( 'NONE', #17025, 1000.000000000000000 ) ;
#5710 = CARTESIAN_POINT ( 'NONE',  ( 11.79490036187186597, -4.501343696292126495, -15.83274364649303578 ) ) ;
#5711 = ORIENTED_EDGE ( 'NONE', *, *, #10696, .F. ) ;
#5712 = CARTESIAN_POINT ( 'NONE',  ( 46.03750000000000142, 34.52875999999999834, -10.31874999999999964 ) ) ;
#5713 = CARTESIAN_POINT ( 'NONE',  ( 12.11059067823646096, 21.69514399574918073, 3.938167792122971633 ) ) ;
#5714 = EDGE_CURVE ( 'NONE', #9371, #2216, #17689, .T. ) ;
#5715 = EDGE_CURVE ( 'NONE', #11228, #9683, #3986, .T. ) ;
#5716 = CARTESIAN_POINT ( 'NONE',  ( 19.79515554403045741, -3.968114999999999615, -10.69562145279641996 ) ) ;
#5717 = AXIS2_PLACEMENT_3D ( 'NONE', #545, #17680, #15600 ) ;
#5718 = CARTESIAN_POINT ( 'NONE',  ( 38.96848998618624904, -7.547609999999999708, -3.934807454472129429 ) ) ;
#5719 = AXIS2_PLACEMENT_3D ( 'NONE', #17605, #12420, #1007 ) ;
#5720 = CIRCLE ( 'NONE', #20894, 1.190625000000000711 ) ;
#5721 = ORIENTED_EDGE ( 'NONE', *, *, #8042, .T. ) ;
#5722 = CARTESIAN_POINT ( 'NONE',  ( -16.73439918454169018, 37.15413452960619622, -25.92417111164088084 ) ) ;
#5723 = CARTESIAN_POINT ( 'NONE',  ( -21.45091887247874851, 40.79338547039380103, -9.992285829511605044 ) ) ;
#5724 = CARTESIAN_POINT ( 'NONE',  ( 11.35915110355360724, 0.1799203519520370387, -16.89710733764713879 ) ) ;
#5725 = DIRECTION ( 'NONE',  ( -0.08420877549337300871, 0.000000000000000000, -0.9964481331860212121 ) ) ;
#5726 = ORIENTED_EDGE ( 'NONE', *, *, #13204, .F. ) ;
#5727 = ORIENTED_EDGE ( 'NONE', *, *, #8029, .F. ) ;
#5728 = AXIS2_PLACEMENT_3D ( 'NONE', #12713, #19438, #11050 ) ;
#5730 = FACE_OUTER_BOUND ( 'NONE', #20356, .T. ) ;
#5729 = CARTESIAN_POINT ( 'NONE',  ( 1.308477177346879960, 18.94235087979956234, 8.980548047580915849 ) ) ;
#5731 = ORIENTED_EDGE ( 'NONE', *, *, #13671, .T. ) ;
#5732 = CARTESIAN_POINT ( 'NONE',  ( 5.486362570609389699, 13.28024286532647658, 7.851790441297502809 ) ) ;
#5733 = VERTEX_POINT ( 'NONE', #2540 ) ;
#5734 = B_SPLINE_CURVE_WITH_KNOTS ( 'NONE', 3,
 ( #4224, #9410, #9302, #12745 ),
 .UNSPECIFIED., .F., .F.,
 ( 4, 4 ),
 ( 0.008329792089495299118, 0.009162609743145318231 ),
 .UNSPECIFIED. ) ;
#5735 = EDGE_LOOP ( 'NONE', ( #5605, #1849, #6831, #6233 ) ) ;
#5736 = EDGE_CURVE ( 'NONE', #10254, #1010, #11869, .T. ) ;
#5737 = CARTESIAN_POINT ( 'NONE',  ( 1.406030455404901236, 13.81240482153004301, 8.014482998805931402 ) ) ;
#5738 = CIRCLE ( 'NONE', #13526, 4.365624999999999645 ) ;
#5739 = VERTEX_POINT ( 'NONE', #4853 ) ;
#5740 = VECTOR ( 'NONE', #8220, 1000.000000000000114 ) ;
#5741 = CIRCLE ( 'NONE', #19498, 1.785937499999998179 ) ;
#5742 = EDGE_CURVE ( 'NONE', #18438, #4597, #6077, .T. ) ;
#5743 = DIRECTION ( 'NONE',  ( 0.9724402360367340181, 0.000000000000000000, -0.2331522835762512846 ) ) ;
#5744 = DIRECTION ( 'NONE',  ( -0.9685006480810791629, 2.034481705827060032E-16, -0.2490110332224850231 ) ) ;
#5745 = CARTESIAN_POINT ( 'NONE',  ( 37.51913901087312553, 42.06303499999999929, -14.58057485080488114 ) ) ;
#5746 = CARTESIAN_POINT ( 'NONE',  ( 1.924744121216944492, 21.16741921860587183, 5.146558987964561460 ) ) ;
#5747 = ORIENTED_EDGE ( 'NONE', *, *, #21637, .F. ) ;
#5748 = CARTESIAN_POINT ( 'NONE',  ( 2.729946285357361280, 19.31779869980666220, 0.8719274852789313801 ) ) ;
#5749 = CARTESIAN_POINT ( 'NONE',  ( 41.45112526417833010, -1.983739999999999837, 7.778260066349530710 ) ) ;
#5750 = CARTESIAN_POINT ( 'NONE',  ( 13.03965183343015610, 21.58187285162961189, 1.970499231081598079 ) ) ;
#5751 = CARTESIAN_POINT ( 'NONE',  ( 18.65312499999999929, 30.56064500000000095, 5.159374999999999822 ) ) ;
#5752 = AXIS2_PLACEMENT_3D ( 'NONE', #9923, #13374, #3309 ) ;
#5753 = ORIENTED_EDGE ( 'NONE', *, *, #17894, .T. ) ;
#5754 = ORIENTED_EDGE ( 'NONE', *, *, #9943, .T. ) ;
#5755 = CARTESIAN_POINT ( 'NONE',  ( 11.27191446706569700, 20.19146305430580313, -2.972894652454601605 ) ) ;
#5757 = CARTESIAN_POINT ( 'NONE',  ( 28.87608719841374949, 30.55334249999999940, -15.73691681567849976 ) ) ;
#5756 = FACE_OUTER_BOUND ( 'NONE', #19984, .T. ) ;
#5758 = CARTESIAN_POINT ( 'NONE',  ( 12.93435681163277629, 11.44283640310037065, 4.674273103487593950 ) ) ;
#5759 = ORIENTED_EDGE ( 'NONE', *, *, #5859, .F. ) ;
#5760 = ORIENTED_EDGE ( 'NONE', *, *, #4364, .F. ) ;
#5761 = CARTESIAN_POINT ( 'NONE',  ( 26.59062499999999929, 5.953125000000000000, 8.731249999999999289 ) ) ;
#5762 = CARTESIAN_POINT ( 'NONE',  ( 7.774415866391942487, 11.36058604623794110, 0.08081017952465485710 ) ) ;
#5763 = CARTESIAN_POINT ( 'NONE',  ( 7.035607835188398163, 12.34291428558256065, 5.584210644256598854 ) ) ;
#5764 = DIRECTION ( 'NONE',  ( -0.2490110332224850509, 0.000000000000000000, 0.9685006480810792739 ) ) ;
#5765 = EDGE_CURVE ( 'NONE', #1238, #2549, #6281, .T. ) ;
#5766 = CARTESIAN_POINT ( 'NONE',  ( 6.035803313514758628, 12.13412562418924878, 1.232330704826734458 ) ) ;
#5767 = ADVANCED_FACE ( 'NONE', ( #1418 ), #13165, .T. ) ;
#5768 = EDGE_CURVE ( 'NONE', #9142, #2020, #4669, .T. ) ;
#5769 = DIRECTION ( 'NONE',  ( -0.000000000000000000, -1.000000000000000000, 0.000000000000000000 ) ) ;
#5770 = AXIS2_PLACEMENT_3D ( 'NONE', #10913, #15801, #5828 ) ;
#5771 = CARTESIAN_POINT ( 'NONE',  ( 11.63353270475617229, 12.58417018233828166, -2.804383768420597445 ) ) ;
#5772 = CARTESIAN_POINT ( 'NONE',  ( -2.256261688646920227, 22.62314500000000095, -0.3933872460174320240 ) ) ;
#5773 = CARTESIAN_POINT ( 'NONE',  ( 4.967848656229971738, 21.41895532286982018, 1.997643190962260284 ) ) ;
#5774 = CARTESIAN_POINT ( 'NONE',  ( 1.576549648455226160, 17.24306997481907899, 9.529489457303672140 ) ) ;
#5775 = AXIS2_PLACEMENT_3D ( 'NONE', #2450, #18427, #5866 ) ;
#5776 = DIRECTION ( 'NONE',  ( 0.6702301885068630005, 0.000000000000000000, 0.7421532822901580895 ) ) ;
#5777 = CARTESIAN_POINT ( 'NONE',  ( 1.950423677167738346, 13.53163558985986192, 0.9959168722820052055 ) ) ;
#5778 = CYLINDRICAL_SURFACE ( 'NONE', #5719, 9.524999999999998579 ) ;
#5779 = CARTESIAN_POINT ( 'NONE',  ( 13.29522536647246511, 1.581453584762025244, -16.25997556760552953 ) ) ;
#5780 = ORIENTED_EDGE ( 'NONE', *, *, #11880, .F. ) ;
#5781 = DIRECTION ( 'NONE',  ( 0.2490110332224836354, 0.000000000000000000, -0.9685006480810794960 ) ) ;
#5782 = CARTESIAN_POINT ( 'NONE',  ( 10.73969208887204019, 10.95696249848220205, 4.001686992780678409 ) ) ;
#5783 = ORIENTED_EDGE ( 'NONE', *, *, #1953, .F. ) ;
#5784 = VECTOR ( 'NONE', #13500, 1000.000000000000114 ) ;
#5785 = CARTESIAN_POINT ( 'NONE',  ( 3.805353748838121053, -14.84248999999999974, -22.18284873352824960 ) ) ;
#5786 = CARTESIAN_POINT ( 'NONE',  ( 11.63141746489545980, 11.77663938069181349, -0.8745901904067018284 ) ) ;
#5787 = CARTESIAN_POINT ( 'NONE',  ( 5.774788405422635940, 19.06000005006808706, -1.475126938916978769 ) ) ;
#5788 = DIRECTION ( 'NONE',  ( 0.2064631973582987667, 0.000000000000000000, -0.9784543669157944601 ) ) ;
#5789 = CARTESIAN_POINT ( 'NONE',  ( 2.415885207217761455, 12.01605003366594104, 3.603415997180536845 ) ) ;
#5790 = ORIENTED_EDGE ( 'NONE', *, *, #14371, .T. ) ;
#5791 = CARTESIAN_POINT ( 'NONE',  ( 28.87608719841374949, 39.28205249999999893, -15.73691681567849976 ) ) ;
#5792 = CARTESIAN_POINT ( 'NONE',  ( 5.089517729310932381, 20.57392463301560426, 2.318340695833992715 ) ) ;
#5793 = EDGE_CURVE ( 'NONE', #1101, #19328, #9709, .T. ) ;
#5794 = CARTESIAN_POINT ( 'NONE',  ( 50.62387473582167274, 0.000000000000000000, -28.41576006634952734 ) ) ;
#5795 = CIRCLE ( 'NONE', #17815, 0.5079999999999963434 ) ;
#5796 = VERTEX_POINT ( 'NONE', #19875 ) ;
#5797 = CARTESIAN_POINT ( 'NONE',  ( 11.33002609776169578, 15.75027095350177397, 6.855137435532622447 ) ) ;
#5798 = VECTOR ( 'NONE', #17681, 1000.000000000000114 ) ;
#5799 = CARTESIAN_POINT ( 'NONE',  ( 11.15970370577760029, 14.44082934938793272, -3.345223894823480038 ) ) ;
#5800 = FACE_OUTER_BOUND ( 'NONE', #8300, .T. ) ;
#5801 = CYLINDRICAL_SURFACE ( 'NONE', #4742, 0.3962399999999998146 ) ;
#5802 = CARTESIAN_POINT ( 'NONE',  ( 4.837794195432601363, 20.03811753756829361, 7.273909691047188097 ) ) ;
#5803 = CARTESIAN_POINT ( 'NONE',  ( 12.30151367325157530, -1.153126200941767543, -16.62801696922743844 ) ) ;
#5804 = DIRECTION ( 'NONE',  ( 0.000000000000000000, 0.000000000000000000, 1.000000000000000000 ) ) ;
#5805 = ORIENTED_EDGE ( 'NONE', *, *, #16191, .T. ) ;
#5806 = CARTESIAN_POINT ( 'NONE',  ( 11.14506973860339478, 16.78189356879117256, 6.798425575953311650 ) ) ;
#5807 = CARTESIAN_POINT ( 'NONE',  ( 10.81988799240761701, 16.27139746542214027, -4.448395456820358085 ) ) ;
#5808 = CIRCLE ( 'NONE', #9333, 0.5080000000000011173 ) ;
#5809 = CARTESIAN_POINT ( 'NONE',  ( 17.95270069355080622, -8.291107314758558999, -14.47941694501537668 ) ) ;
#5810 = ORIENTED_EDGE ( 'NONE', *, *, #5314, .F. ) ;
#5811 = CARTESIAN_POINT ( 'NONE',  ( 9.405431565759853285, 13.38381860909070653, -1.897411705095320089 ) ) ;
#5812 = CARTESIAN_POINT ( 'NONE',  ( 1.075305989013234598, 18.45120109744945225, 8.266748288633882780 ) ) ;
#5814 = DIRECTION ( 'NONE',  ( -0.8943161143440100380, 0.000000000000000000, -0.4474356798743612806 ) ) ;
#5813 = CARTESIAN_POINT ( 'NONE',  ( -0.3990962785833974680, 17.28679025579738138, 0.5365138910678359796 ) ) ;
#5815 = ORIENTED_EDGE ( 'NONE', *, *, #641, .T. ) ;
#5816 = CARTESIAN_POINT ( 'NONE',  ( 34.38097451710952868, 32.54502000000000095, 0.2081255904771098786 ) ) ;
#5817 = EDGE_CURVE ( 'NONE', #2994, #6208, #14939, .T. ) ;
#5818 = CARTESIAN_POINT ( 'NONE',  ( 39.38301085650398647, -7.397690232646351838, -3.502300841008181287 ) ) ;
#5819 = EDGE_LOOP ( 'NONE', ( #11774, #18519, #5452, #7970 ) ) ;
#5820 = CARTESIAN_POINT ( 'NONE',  ( 19.51141091471011180, 2.770822500000000854, -1.622220754415315547 ) ) ;
#5821 = CARTESIAN_POINT ( 'NONE',  ( 17.43744253143330525, -7.133763992443639346, -14.52515173542417593 ) ) ;
#5822 = ORIENTED_EDGE ( 'NONE', *, *, #6411, .F. ) ;
#5823 = LINE ( 'NONE', #17548, #806 ) ;
#5824 = DIRECTION ( 'NONE',  ( -0.2064631973582987667, 0.000000000000000000, 0.9784543669157944601 ) ) ;
#5825 = AXIS2_PLACEMENT_3D ( 'NONE', #11835, #6853, #17136 ) ;
#5826 = DIRECTION ( 'NONE',  ( -0.6702301885068630005, 0.000000000000000000, -0.7421532822901579785 ) ) ;
#5827 = ORIENTED_EDGE ( 'NONE', *, *, #21445, .F. ) ;
#5828 = DIRECTION ( 'NONE',  ( -0.9790635044817342925, 0.000000000000000000, 0.2035550397114870846 ) ) ;
#5829 = CARTESIAN_POINT ( 'NONE',  ( -1.880134707694870011, 12.30439499999999953, 7.779750394130780400 ) ) ;
#5830 = ORIENTED_EDGE ( 'NONE', *, *, #10058, .T. ) ;
#5831 = ORIENTED_EDGE ( 'NONE', *, *, #7365, .T. ) ;
#5832 = CARTESIAN_POINT ( 'NONE',  ( 2.484165171653412330, 11.21351766718956178, 3.437652806735580935 ) ) ;
#5833 = VERTEX_POINT ( 'NONE', #19760 ) ;
#5834 = CARTESIAN_POINT ( 'NONE',  ( 4.865075149428808032, 11.25209086740643016, 5.008807926723467752 ) ) ;
#5835 = ORIENTED_EDGE ( 'NONE', *, *, #9023, .T. ) ;
#5836 = EDGE_CURVE ( 'NONE', #12549, #304, #20532, .T. ) ;
#5837 = ORIENTED_EDGE ( 'NONE', *, *, #11133, .F. ) ;
#5838 = EDGE_CURVE ( 'NONE', #1190, #2509, #18432, .T. ) ;
#5839 = CARTESIAN_POINT ( 'NONE',  ( 1.385753006902628703, 13.65946455019744299, 7.893527135823292795 ) ) ;
#5840 = EDGE_LOOP ( 'NONE', ( #13771, #19288, #5462, #66 ) ) ;
#5841 = CARTESIAN_POINT ( 'NONE',  ( 26.59062499999999929, 5.953125000000000000, 10.71562499999999929 ) ) ;
#5842 = CARTESIAN_POINT ( 'NONE',  ( 29.64606458365116737, -6.752907499999998286, -15.53894806404596096 ) ) ;
#5843 = DIRECTION ( 'NONE',  ( 0.000000000000000000, 1.000000000000000000, 0.000000000000000000 ) ) ;
#5844 = CARTESIAN_POINT ( 'NONE',  ( 3.588180185287924484, 13.77383989023144117, 8.530597361598315942 ) ) ;
#5845 = ORIENTED_EDGE ( 'NONE', *, *, #6825, .F. ) ;
#5846 = DIRECTION ( 'NONE',  ( 0.9037041334408598692, 0.3596272420165190220, 0.2323512126103423059 ) ) ;
#5847 = DIRECTION ( 'NONE',  ( -0.000000000000000000, -1.000000000000000000, 0.000000000000000000 ) ) ;
#5848 = DIRECTION ( 'NONE',  ( 0.000000000000000000, -1.000000000000000000, 0.000000000000000000 ) ) ;
#5849 = EDGE_CURVE ( 'NONE', #6840, #93, #20183, .T. ) ;
#5850 = ORIENTED_EDGE ( 'NONE', *, *, #15998, .T. ) ;
#5851 = EDGE_LOOP ( 'NONE', ( #14339, #10537, #9365, #3438, #9246, #20222 ) ) ;
#5852 = CARTESIAN_POINT ( 'NONE',  ( 7.122862576751088248, 21.40982604368873865, 3.348050232907604951 ) ) ;
#5854 = DIRECTION ( 'NONE',  ( -0.2490110332224855227, 0.000000000000000000, 0.9685006480810791629 ) ) ;
#5853 = DIRECTION ( 'NONE',  ( 0.000000000000000000, 1.000000000000000000, 0.000000000000000000 ) ) ;
#5855 = CARTESIAN_POINT ( 'NONE',  ( 12.60979462320922373, 10.71893859347252231, 3.290081565980131906 ) ) ;
#5856 = ORIENTED_EDGE ( 'NONE', *, *, #17317, .T. ) ;
#5857 = VERTEX_POINT ( 'NONE', #21319 ) ;
#5858 = CARTESIAN_POINT ( 'NONE',  ( 29.64606458365116737, -7.547927499999999235, -15.53894806404596096 ) ) ;
#5859 = EDGE_CURVE ( 'NONE', #7283, #14216, #10680, .T. ) ;
#5860 = CARTESIAN_POINT ( 'NONE',  ( 7.526575487049647961, 18.64928636511069371, -2.428959993994535882 ) ) ;
#5861 = CARTESIAN_POINT ( 'NONE',  ( 6.704184490690651366, 11.71035962591412272, 4.082957847732187062 ) ) ;
#5862 = CARTESIAN_POINT ( 'NONE',  ( 43.49132289107146931, 34.52875999999999834, 4.686923926377883021 ) ) ;
#5863 = EDGE_CURVE ( 'NONE', #13820, #7283, #13276, .T. ) ;
#5864 = CARTESIAN_POINT ( 'NONE',  ( 7.067667105230608371, 20.80763019527516988, 1.945974362385073819 ) ) ;
#5865 = CARTESIAN_POINT ( 'NONE',  ( 2.447833637063231205, 19.89874561968573374, 6.469289142455495245 ) ) ;
#5866 = DIRECTION ( 'NONE',  ( 0.9724402360367340181, 0.000000000000000000, -0.2331522835762512846 ) ) ;
#5867 = CARTESIAN_POINT ( 'NONE',  ( 8.720760638157020850, 10.73926345162572105, 3.665552357571379538 ) ) ;
#5868 = LINE ( 'NONE', #12632, #7038 ) ;
#5869 = CARTESIAN_POINT ( 'NONE',  ( 7.415316962347603180, 12.98226186039768137, 7.408690243710602807 ) ) ;
#5870 = CARTESIAN_POINT ( 'NONE',  ( 0.7102513561496924810, 20.31959456549100906, 7.525625334632009000 ) ) ;
#5871 = LINE ( 'NONE', #12863, #20210 ) ;
#5872 = CARTESIAN_POINT ( 'NONE',  ( 0.1976490688386850214, 20.17752205389220066, 6.189897254476726118 ) ) ;
#5873 = CARTESIAN_POINT ( 'NONE',  ( 24.60624999999999929, 16.27314499999999953, 8.731249999999999289 ) ) ;
#5874 = DIRECTION ( 'NONE',  ( -0.9964481331860213231, 0.000000000000000000, 0.08420877549337293932 ) ) ;
#5875 = CARTESIAN_POINT ( 'NONE',  ( 16.83076340656427305, 2.188335711206311984, -15.21158537076933825 ) ) ;
#5876 = EDGE_CURVE ( 'NONE', #7268, #9462, #4427, .T. ) ;
#5877 = ORIENTED_EDGE ( 'NONE', *, *, #18022, .T. ) ;
#5878 = EDGE_CURVE ( 'NONE', #8651, #7667, #11594, .T. ) ;
#5879 = DIRECTION ( 'NONE',  ( 0.000000000000000000, -1.000000000000000000, 0.000000000000000000 ) ) ;
#5880 = ADVANCED_FACE ( 'NONE', ( #17906 ), #19982, .T. ) ;
#5881 = CARTESIAN_POINT ( 'NONE',  ( 10.02755535553010624, 10.65547162720833185, 1.022515237104560271 ) ) ;
#5882 = ORIENTED_EDGE ( 'NONE', *, *, #14010, .T. ) ;
#5883 = CARTESIAN_POINT ( 'NONE',  ( 26.34068084182479907, 1.140633240613131871, 10.52776784000260157 ) ) ;
#5884 = CARTESIAN_POINT ( 'NONE',  ( 5.810244688662751678, 11.73040477827100325, 0.3453541907369687136 ) ) ;
#5885 = DIRECTION ( 'NONE',  ( 0.9579671649362033747, 0.000000000000000000, -0.2868778675745010664 ) ) ;
#5886 = CARTESIAN_POINT ( 'NONE',  ( 2.012643648797029616, 17.94014877828372079, 0.2841994374236595511 ) ) ;
#5887 = ORIENTED_EDGE ( 'NONE', *, *, #14248, .F. ) ;
#5888 = CARTESIAN_POINT ( 'NONE',  ( 36.51250000000000284, 0.000000000000000000, -10.31875000000000142 ) ) ;
#5889 = VECTOR ( 'NONE', #8278, 1000.000000000000000 ) ;
#5890 = DIRECTION ( 'NONE',  ( 0.000000000000000000, 1.000000000000000000, 0.000000000000000000 ) ) ;
#5891 = ORIENTED_EDGE ( 'NONE', *, *, #674, .T. ) ;
#5892 = CARTESIAN_POINT ( 'NONE',  ( 5.774107441413635300, 17.24227063501358614, -1.439737884917017707 ) ) ;
#5893 = CARTESIAN_POINT ( 'NONE',  ( 4.924203502439124414, 18.75546692123623060, 7.326012498920505323 ) ) ;
#5894 = CARTESIAN_POINT ( 'NONE',  ( 9.588774839205283840, 12.37377145998696193, -1.094828636744461292 ) ) ;
#5895 = CARTESIAN_POINT ( 'NONE',  ( 71.03963378001139972, 1.984375000000000000, -10.54138470677948014 ) ) ;
#5896 = CARTESIAN_POINT ( 'NONE',  ( 9.262381024405307528, 30.63641399982339308, -21.59935919086856515 ) ) ;
#5897 = CARTESIAN_POINT ( 'NONE',  ( 5.464785416199259060, 17.37627409491906505, 8.697631989696647636 ) ) ;
#5898 = EDGE_CURVE ( 'NONE', #21060, #9547, #6397, .T. ) ;
#5899 = EDGE_CURVE ( 'NONE', #6208, #14041, #1484, .T. ) ;
#5900 = CARTESIAN_POINT ( 'NONE',  ( 52.96420052373725440, 32.54502000000000095, 7.017842122255405712 ) ) ;
#5901 = VECTOR ( 'NONE', #16551, 1000.000000000000000 ) ;
#5902 = ORIENTED_EDGE ( 'NONE', *, *, #10301, .F. ) ;
#5903 = CARTESIAN_POINT ( 'NONE',  ( 6.392593417591551308, 10.79308423060320088, 3.256129757715929163 ) ) ;
#5904 = CARTESIAN_POINT ( 'NONE',  ( 52.32428405346736611, 39.49694501955431036, -17.47444899681294217 ) ) ;
#5905 = ORIENTED_EDGE ( 'NONE', *, *, #3028, .F. ) ;
#5906 = CARTESIAN_POINT ( 'NONE',  ( 10.22638260995712400, 20.36150965861552464, -0.9086538386368623321 ) ) ;
#5907 = CARTESIAN_POINT ( 'NONE',  ( 53.10322573897614973, 37.69740999999999786, -16.70632925929051638 ) ) ;
#5908 = CARTESIAN_POINT ( 'NONE',  ( 0.8501141161861881512, 19.12429843616597580, 7.755429456263986054 ) ) ;
#5910 = DIRECTION ( 'NONE',  ( 0.000000000000000000, 1.000000000000000000, 0.000000000000000000 ) ) ;
#5909 = CARTESIAN_POINT ( 'NONE',  ( 2.439223677983356708, 11.63542902183100125, 5.280048492248608838 ) ) ;
#5911 = VERTEX_POINT ( 'NONE', #10475 ) ;
#5912 = DIRECTION ( 'NONE',  ( 0.000000000000000000, 1.000000000000000000, 0.000000000000000000 ) ) ;
#5913 = CARTESIAN_POINT ( 'NONE',  ( 39.47917727842295932, -7.309119366952678831, -3.410336071361241839 ) ) ;
#5914 = VERTEX_POINT ( 'NONE', #15144 ) ;
#5915 = CARTESIAN_POINT ( 'NONE',  ( 38.96848998618624904, 37.69740999999999786, -3.934807454472129429 ) ) ;
#5916 = CARTESIAN_POINT ( 'NONE',  ( 0.03622098100764838124, 15.71836236879072679, 0.8515907948898381319 ) ) ;
#5917 = CARTESIAN_POINT ( 'NONE',  ( 19.50624135474398457, -0.8684152889774677808, -15.55849431363919599 ) ) ;
#5918 = ORIENTED_EDGE ( 'NONE', *, *, #16412, .T. ) ;
#5919 = DIRECTION ( 'NONE',  ( 0.2868778675745004558, 0.000000000000000000, 0.9579671649362035968 ) ) ;
#5920 = CARTESIAN_POINT ( 'NONE',  ( 11.00068862475037790, 16.27139746542210119, -4.502538961693060671 ) ) ;
#5921 = EDGE_CURVE ( 'NONE', #17008, #1449, #13868, .T. ) ;
#5922 = CARTESIAN_POINT ( 'NONE',  ( -17.46249999999999858, -1.587500000000002132, 0.000000000000000000 ) ) ;
#5923 = VERTEX_POINT ( 'NONE', #3311 ) ;
#5924 = PLANE ( 'NONE',  #17791 ) ;
#5926 = DIRECTION ( 'NONE',  ( -0.2868778675745010664, 0.000000000000000000, -0.9579671649362032637 ) ) ;
#5925 = DIRECTION ( 'NONE',  ( 0.2490110332224836354, 0.000000000000000000, -0.9685006480810794960 ) ) ;
#5927 = VERTEX_POINT ( 'NONE', #8371 ) ;
#5928 = ORIENTED_EDGE ( 'NONE', *, *, #13438, .F. ) ;
#5929 = CARTESIAN_POINT ( 'NONE',  ( 20.46463427092750464, -6.006569699063351919, -13.84993367446087476 ) ) ;
#5931 = CARTESIAN_POINT ( 'NONE',  ( 14.33584040382675262, 24.59767750000000319, -46.84351661546690337 ) ) ;
#5930 = CARTESIAN_POINT ( 'NONE',  ( 1.805619654075212965, 13.02087111295804256, 0.3827243396642013851 ) ) ;
#5932 = ORIENTED_EDGE ( 'NONE', *, *, #7853, .T. ) ;
#5933 = CARTESIAN_POINT ( 'NONE',  ( 3.861727869702078042, 18.73760406805453371, -0.8916021778709736223 ) ) ;
#5934 = VERTEX_POINT ( 'NONE', #15371 ) ;
#5935 = ORIENTED_EDGE ( 'NONE', *, *, #3642, .T. ) ;
#5936 = ORIENTED_EDGE ( 'NONE', *, *, #14597, .F. ) ;
#5937 = CARTESIAN_POINT ( 'NONE',  ( 2.889068357235882623, 12.18047855553292713, 5.318317885449051374 ) ) ;
#5939 = MANIFOLD_SOLID_BREP ( 'Stock-MAS-676-1', #5704 ) ;
#5938 = AXIS2_PLACEMENT_3D ( 'NONE', #20588, #371, #18504 ) ;
#5940 = DIRECTION ( 'NONE',  ( 0.7334850928793767988, -0.6768732144311027099, -0.06198604769976990420 ) ) ;
#5941 = CARTESIAN_POINT ( 'NONE',  ( 39.80287034594652340, 38.26567781475652907, -3.117403183957448309 ) ) ;
#5942 = FACE_OUTER_BOUND ( 'NONE', #20778, .T. ) ;
#5943 = CARTESIAN_POINT ( 'NONE',  ( 31.05388211198297554, -1.983739999999999837, -15.23127950648024331 ) ) ;
#5944 = CARTESIAN_POINT ( 'NONE',  ( 2.377763845684053745, 11.40282469389570075, 3.054462267276081278 ) ) ;
#5945 = EDGE_CURVE ( 'NONE', #7624, #8950, #14929, .T. ) ;
#5946 = ORIENTED_EDGE ( 'NONE', *, *, #21824, .F. ) ;
#5947 = DIRECTION ( 'NONE',  ( 0.000000000000000000, -1.000000000000000000, -0.000000000000000000 ) ) ;
#5948 = DIRECTION ( 'NONE',  ( 0.000000000000000000, -1.000000000000000000, 0.000000000000000000 ) ) ;
#5949 = CARTESIAN_POINT ( 'NONE',  ( 29.64606458365116737, -7.547927499999999235, -15.53894806404596096 ) ) ;
#5950 = DIRECTION ( 'NONE',  ( 0.1878280753562735217, 0.000000000000000000, 0.9822019212503905194 ) ) ;
#5951 = CARTESIAN_POINT ( 'NONE',  ( 21.43124999999999858, 16.27314499999999953, 8.731249999999999289 ) ) ;
#5952 = ORIENTED_EDGE ( 'NONE', *, *, #20286, .T. ) ;
#5953 = VERTEX_POINT ( 'NONE', #20083 ) ;
#5954 = CARTESIAN_POINT ( 'NONE',  ( 6.447884206030225940, 11.65642365002708125, 5.039460170731214106 ) ) ;
#5956 = LINE ( 'NONE', #9163, #15251 ) ;
#5955 = CARTESIAN_POINT ( 'NONE',  ( -16.07247711516169275, 35.13319853559599437, -10.44681224123558039 ) ) ;
#5957 = CARTESIAN_POINT ( 'NONE',  ( 12.85806460298763021, 11.22509623584751282, 4.343794590431158120 ) ) ;
#5958 = ORIENTED_EDGE ( 'NONE', *, *, #4769, .F. ) ;
#5959 = VERTEX_POINT ( 'NONE', #18644 ) ;
#5960 = DIRECTION ( 'NONE',  ( 0.000000000000000000, 1.000000000000000000, 0.000000000000000000 ) ) ;
#5961 = AXIS2_PLACEMENT_3D ( 'NONE', #1309, #18232, #19983 ) ;
#5962 = CARTESIAN_POINT ( 'NONE',  ( 7.267304438700130653, 16.63416352659407238, -2.882144068962717576 ) ) ;
#5963 = FACE_OUTER_BOUND ( 'NONE', #9662, .T. ) ;
#5964 = CARTESIAN_POINT ( 'NONE',  ( 6.892979284088748493, 20.66668035358058120, 1.484166371361514747 ) ) ;
#5965 = CARTESIAN_POINT ( 'NONE',  ( 54.61912012054379062, -6.356984999999999886, -13.79062155615056362 ) ) ;
#5966 = ADVANCED_FACE ( 'NONE', ( #6834, #18759 ), #3740, .T. ) ;
#5967 = TOROIDAL_SURFACE ( 'NONE', #19387, 4.961572499999999941, 0.3962400000000000366 ) ;
#5968 = CARTESIAN_POINT ( 'NONE',  ( 13.86187374551126439, 22.11716190621255862, 2.323971484891082184 ) ) ;
#5969 = CARTESIAN_POINT ( 'NONE',  ( 50.29383871662588490, 34.52875999999999834, -28.02957329025317179 ) ) ;
#5970 = CARTESIAN_POINT ( 'NONE',  ( 0.8098354902157162138, 20.20131944153736114, 7.871963320744100656 ) ) ;
#5971 = CARTESIAN_POINT ( 'NONE',  ( 1.655340346233492355, 13.96895574127920625, 9.020042064985599239 ) ) ;
#5972 = ADVANCED_FACE ( 'NONE', ( #16791, #20196, #10251, #5066, #21758 ), #17115, .F. ) ;
#5973 = EDGE_CURVE ( 'NONE', #15045, #7695, #18546, .T. ) ;
#5974 = ADVANCED_FACE ( 'NONE', ( #17217 ), #13594, .F. ) ;
#5975 = CARTESIAN_POINT ( 'NONE',  ( 11.75439013559175017, 128.5105379999999968, 4.331204221326972359 ) ) ;
#5976 = CARTESIAN_POINT ( 'NONE',  ( 0.1177374572251341928, 17.19689764357661943, 0.7940873122000081663 ) ) ;
#5977 = DIRECTION ( 'NONE',  ( 0.6702301885068628895, 0.000000000000000000, 0.7421532822901579785 ) ) ;
#5978 = PLANE ( 'NONE',  #21243 ) ;
#5979 = CARTESIAN_POINT ( 'NONE',  ( 12.63934909048015598, -7.435355452895607620, -15.59063177402284239 ) ) ;
#5980 = VERTEX_POINT ( 'NONE', #1738 ) ;
#5981 = DIRECTION ( 'NONE',  ( 0.000000000000000000, 1.000000000000000000, 0.000000000000000000 ) ) ;
#5982 = AXIS2_PLACEMENT_3D ( 'NONE', #13585, #18751, #13471 ) ;
#5983 = LINE ( 'NONE', #8302, #7824 ) ;
#5984 = CARTESIAN_POINT ( 'NONE',  ( 10.56390221082172687, 10.71761206645349240, 3.260385432885468227 ) ) ;
#5985 = ORIENTED_EDGE ( 'NONE', *, *, #2025, .F. ) ;
#5986 = AXIS2_PLACEMENT_3D ( 'NONE', #15276, #13290, #11608 ) ;
#5987 = CARTESIAN_POINT ( 'NONE',  ( 21.94726064351640105, 0.7124538231385260101, 10.25520621805301857 ) ) ;
#5988 = CARTESIAN_POINT ( 'NONE',  ( 12.30618434154357566, 20.85343389055401175, -1.024261053597833371 ) ) ;
#5989 = CARTESIAN_POINT ( 'NONE',  ( 6.049413308899639574, 11.22004793005951306, 1.386673510691023292 ) ) ;
#5990 = DIRECTION ( 'NONE',  ( 0.000000000000000000, 0.000000000000000000, -1.000000000000000000 ) ) ;
#5991 = ORIENTED_EDGE ( 'NONE', *, *, #12328, .T. ) ;
#5992 = SURFACE_SIDE_STYLE ('',( #7986 ) ) ;
#5993 = AXIS2_PLACEMENT_3D ( 'NONE', #940, #2608, #5814 ) ;
#5994 = DIRECTION ( 'NONE',  ( 0.8667647648559581031, 0.000000000000000000, 0.4987171968201974948 ) ) ;
#5995 = ADVANCED_FACE ( 'NONE', ( #8696 ), #15475, .F. ) ;
#5996 = ORIENTED_EDGE ( 'NONE', *, *, #8406, .T. ) ;
#5997 = CARTESIAN_POINT ( 'NONE',  ( 8.886489067368289696, 11.45164960235222118, 3.463840564905101171 ) ) ;
#5998 = CIRCLE ( 'NONE', #11659, 1.587500000000001688 ) ;
#5999 = VECTOR ( 'NONE', #15219, 1000.000000000000114 ) ;
#6000 = CARTESIAN_POINT ( 'NONE',  ( 7.863974401675383419, 12.04767321495844179, 0.2472099257450396381 ) ) ;
#6001 = DIRECTION ( 'NONE',  ( -1.000000000000000000, 0.000000000000000000, 0.000000000000000000 ) ) ;
#6002 = VECTOR ( 'NONE', #7334, 1000.000000000000000 ) ;
#6003 = LINE ( 'NONE', #9651, #13198 ) ;
#6004 = EDGE_CURVE ( 'NONE', #337, #8462, #12146, .T. ) ;
#6005 = EDGE_CURVE ( 'NONE', #11084, #14947, #7484, .T. ) ;
#6006 = CYLINDRICAL_SURFACE ( 'NONE', #7923, 30.16250000000000142 ) ;
#6007 = DIRECTION ( 'NONE',  ( 0.000000000000000000, -1.000000000000000000, -0.000000000000000000 ) ) ;
#6008 = CARTESIAN_POINT ( 'NONE',  ( 5.020040770389102569, 19.52513284903354673, 7.730226423647035716 ) ) ;
#6009 = FACE_OUTER_BOUND ( 'NONE', #4581, .T. ) ;
#6010 = AXIS2_PLACEMENT_3D ( 'NONE', #3447, #10180, #18477 ) ;
#6011 = VERTEX_POINT ( 'NONE', #848 ) ;
#6012 = FACE_OUTER_BOUND ( 'NONE', #8228, .T. ) ;
#6013 = ORIENTED_EDGE ( 'NONE', *, *, #2901, .T. ) ;
#6014 = CARTESIAN_POINT ( 'NONE',  ( 9.792942318191714790, 19.23395335097719538, -1.995198763412909804 ) ) ;
#6015 = CARTESIAN_POINT ( 'NONE',  ( 30.33489826846160398, 32.54502000000000095, -2.417033907079745525 ) ) ;
#6016 = CARTESIAN_POINT ( 'NONE',  ( 1.255833685023748370, 17.68435013880464624, 8.631050028349431358 ) ) ;
#6017 = CARTESIAN_POINT ( 'NONE',  ( 14.09647384216111377, -8.336694694684233298, -16.02083815639807440 ) ) ;
#6018 = CIRCLE ( 'NONE', #20798, 0.7950199999999988387 ) ;
#6019 = CARTESIAN_POINT ( 'NONE',  ( 5.052911015069207146, 14.03105527214651715, 8.089863925655100374 ) ) ;
#6020 = ORIENTED_EDGE ( 'NONE', *, *, #882, .T. ) ;
#6021 = CARTESIAN_POINT ( 'NONE',  ( 5.447351731530780228, 32.54502000000000095, 0.8930339070797439494 ) ) ;
#6022 = CYLINDRICAL_SURFACE ( 'NONE', #9479, 0.7950200000000003930 ) ;
#6023 = ORIENTED_EDGE ( 'NONE', *, *, #7365, .F. ) ;
#6024 = FACE_OUTER_BOUND ( 'NONE', #1194, .T. ) ;
#6025 = EDGE_CURVE ( 'NONE', #2096, #17518, #21175, .T. ) ;
#6026 = CIRCLE ( 'NONE', #20149, 0.7950199999999993938 ) ;
#6027 = EDGE_CURVE ( 'NONE', #16499, #3464, #2400, .T. ) ;
#6028 = EDGE_CURVE ( 'NONE', #288, #12389, #7133, .T. ) ;
#6029 = VECTOR ( 'NONE', #14501, 1000.000000000000000 ) ;
#6030 = CARTESIAN_POINT ( 'NONE',  ( 19.38382740634625279, -5.839277843515219502, -15.34916028355615225 ) ) ;
#6031 = VERTEX_POINT ( 'NONE', #11230 ) ;
#6032 = CARTESIAN_POINT ( 'NONE',  ( 8.599231060378546232, 19.63015825768726330, 6.053049467817567475 ) ) ;
#6033 = VECTOR ( 'NONE', #21633, 1000.000000000000000 ) ;
#6034 = CARTESIAN_POINT ( 'NONE',  ( 37.51913901087312553, 42.06303499999999929, -14.58057485080488114 ) ) ;
#6035 = CIRCLE ( 'NONE', #10637, 1.190625000000001155 ) ;
#6036 = CARTESIAN_POINT ( 'NONE',  ( 29.36874999999999858, 0.000000000000000000, -10.31874999999999964 ) ) ;
#6037 = ORIENTED_EDGE ( 'NONE', *, *, #6004, .F. ) ;
#6038 = DIRECTION ( 'NONE',  ( 0.9636276526537417286, 0.000000000000000000, -0.2672484743474499158 ) ) ;
#6039 = DIRECTION ( 'NONE',  ( 0.05085730733808393328, 0.000000000000000000, -0.9987059298363656357 ) ) ;
#6040 = ORIENTED_EDGE ( 'NONE', *, *, #437, .T. ) ;
#6041 = EDGE_LOOP ( 'NONE', ( #17010, #331, #2295, #9332 ) ) ;
#6042 = AXIS2_PLACEMENT_3D ( 'NONE', #17973, #1268, #1369 ) ;
#6043 = CARTESIAN_POINT ( 'NONE',  ( 39.93069333242032570, 38.88803500000010160, -3.008993689095761148 ) ) ;
#6045 = CARTESIAN_POINT ( 'NONE',  ( 48.58367710892853353, 34.52875999999999834, -25.32442392637788231 ) ) ;
#6044 = CARTESIAN_POINT ( 'NONE',  ( 4.684843972026743408, 20.53916262649988056, 6.840992517925734262 ) ) ;
#6046 = EDGE_LOOP ( 'NONE', ( #14554, #19961 ) ) ;
#6047 = CARTESIAN_POINT ( 'NONE',  ( 3.552288670928100078, 16.45067739432806064, -1.423831345796362946 ) ) ;
#6048 = ORIENTED_EDGE ( 'NONE', *, *, #1833, .F. ) ;
#6049 = AXIS2_PLACEMENT_3D ( 'NONE', #109, #5093, #11731 ) ;
#6050 = VERTEX_POINT ( 'NONE', #19625 ) ;
#6051 = VECTOR ( 'NONE', #16500, 1000.000000000000000 ) ;
#6052 = CARTESIAN_POINT ( 'NONE',  ( 0.9277841963642122769, 12.28846772247859498, 5.618827124256060124 ) ) ;
#6053 = EDGE_CURVE ( 'NONE', #17565, #13169, #7370, .T. ) ;
#6054 = VERTEX_POINT ( 'NONE', #16447 ) ;
#6055 = VECTOR ( 'NONE', #12866, 1000.000000000000114 ) ;
#6056 = CIRCLE ( 'NONE', #21244, 0.7950200000000003930 ) ;
#6057 = DIRECTION ( 'NONE',  ( 0.9790635044817342925, 0.000000000000000000, -0.2035550397114870569 ) ) ;
#6058 = DIRECTION ( 'NONE',  ( -0.9579671649362033747, 0.000000000000000000, 0.2868778675745011220 ) ) ;
#6059 = CARTESIAN_POINT ( 'NONE',  ( -46.55710204590916135, -8.889364999999999739, -7.870588902259476605 ) ) ;
#6060 = CARTESIAN_POINT ( 'NONE',  ( -20.63749999999999929, 16.27314499999999953, 10.71562499999999929 ) ) ;
#6061 = CARTESIAN_POINT ( 'NONE',  ( 3.621953361605184885, 14.18517595478938098, 8.745819149335433806 ) ) ;
#6062 = CIRCLE ( 'NONE', #19497, 3.770312499999998845 ) ;
#6063 = VERTEX_POINT ( 'NONE', #20049 ) ;
#6064 = DIRECTION ( 'NONE',  ( 0.9784543669157944601, -0.000000000000000000, 0.2064631973582987945 ) ) ;
#6065 = CARTESIAN_POINT ( 'NONE',  ( 46.03750000000000142, 1.984375000000000000, -10.31874999999999964 ) ) ;
#6066 = CARTESIAN_POINT ( 'NONE',  ( 2.492193568723835462, 5.548947500000001476, -24.56873394466936134 ) ) ;
#6067 = DIRECTION ( 'NONE',  ( -0.9987059298363657467, 0.000000000000000000, -0.05085730733808445370 ) ) ;
#6068 = ORIENTED_EDGE ( 'NONE', *, *, #16161, .F. ) ;
#6069 = ORIENTED_EDGE ( 'NONE', *, *, #14771, .T. ) ;
#6070 = CARTESIAN_POINT ( 'NONE',  ( 9.435867950683245908, 21.13787900135836395, 3.521159264218552742 ) ) ;
#6072 = CARTESIAN_POINT ( 'NONE',  ( 4.766637503084914407, -6.752907499999998286, -3.239749061574506150 ) ) ;
#6071 = CARTESIAN_POINT ( 'NONE',  ( 8.505511374756364873, -3.966527499999997097, -20.97439202360551747 ) ) ;
#6073 = CARTESIAN_POINT ( 'NONE',  ( 11.16014847406012223, 18.33592708871418608, -4.033227821418477355 ) ) ;
#6074 = VERTEX_POINT ( 'NONE', #4719 ) ;
#6075 = ORIENTED_EDGE ( 'NONE', *, *, #1271, .F. ) ;
#6076 = CARTESIAN_POINT ( 'NONE',  ( 14.13556150701963254, -0.7997824999999986195, -46.89501028779991287 ) ) ;
#6077 = CIRCLE ( 'NONE', #7848, 0.7950200000000011702 ) ;
#6078 = CARTESIAN_POINT ( 'NONE',  ( 8.166405835557249304, 10.80616279181379014, 1.748811918552366729 ) ) ;
#6079 = CARTESIAN_POINT ( 'NONE',  ( 43.49132289107146931, 0.000000000000000000, 4.686923926377883021 ) ) ;
#6080 = CARTESIAN_POINT ( 'NONE',  ( 7.219217501582479102, 20.87764444342654357, 2.348948422008501957 ) ) ;
#6081 = ADVANCED_FACE ( 'NONE', ( #10112 ), #19843, .T. ) ;
#6082 = VECTOR ( 'NONE', #11868, 1000.000000000000000 ) ;
#6083 = CARTESIAN_POINT ( 'NONE',  ( 2.724573480716647289, 19.38658690530843742, 7.155403551711358112 ) ) ;
#6084 = CARTESIAN_POINT ( 'NONE',  ( 10.87431863107423169, 10.89466173679246097, 4.149793331543699004 ) ) ;
#6085 = EDGE_CURVE ( 'NONE', #21393, #10995, #6026, .T. ) ;
#6086 = CIRCLE ( 'NONE', #12102, 30.16249999999998366 ) ;
#6087 = DIRECTION ( 'NONE',  ( 0.000000000000000000, 1.000000000000000000, 0.000000000000000000 ) ) ;
#6088 = CARTESIAN_POINT ( 'NONE',  ( 29.19635173153840313, 32.54502000000000095, -6.218966092919240296 ) ) ;
#6089 = CARTESIAN_POINT ( 'NONE',  ( 12.62386444219163373, 19.43957250000000059, -17.86660850434754266 ) ) ;
#6090 = CARTESIAN_POINT ( 'NONE',  ( 1.613076528681359756, 14.62668795976242642, -0.4927809465211088202 ) ) ;
#6091 = CARTESIAN_POINT ( 'NONE',  ( 1.389669449877557472, 12.36033839947706170, 7.643082816218980113 ) ) ;
#6092 = CARTESIAN_POINT ( 'NONE',  ( 49.72033008250774344, 34.52875999999999124, -2.687827786179598277 ) ) ;
#6093 = CARTESIAN_POINT ( 'NONE',  ( 6.659626489177622233, 11.71104153968872197, 4.096152728507711949 ) ) ;
#6094 = DIRECTION ( 'NONE',  ( 1.000000000000000000, 0.000000000000000000, 0.000000000000000000 ) ) ;
#6095 = CARTESIAN_POINT ( 'NONE',  ( 11.81489480681374715, -4.423560566030090513, -15.68132100509055782 ) ) ;
#6096 = CARTESIAN_POINT ( 'NONE',  ( 16.27231063047230464, -8.394727124024923270, -14.79989961003369814 ) ) ;
#6097 = VERTEX_POINT ( 'NONE', #20154 ) ;
#6098 = CARTESIAN_POINT ( 'NONE',  ( 53.46798503507454825, 0.000000000000000000, 6.304111036318381878 ) ) ;
#6099 = AXIS2_PLACEMENT_3D ( 'NONE', #15, #6765, #13641 ) ;
#6100 = CARTESIAN_POINT ( 'NONE',  ( 11.03847332581440277, 11.68029354362261252, 5.291968781390675503 ) ) ;
#6101 = ORIENTED_EDGE ( 'NONE', *, *, #14696, .F. ) ;
#6102 = CARTESIAN_POINT ( 'NONE',  ( 27.72321311043520353, 1.355051563794170022, 10.61353820125299841 ) ) ;
#6103 = CARTESIAN_POINT ( 'NONE',  ( 5.712404053886056765, 18.78909992803161444, -1.619831271828931829 ) ) ;
#6104 = FACE_OUTER_BOUND ( 'NONE', #13488, .T. ) ;
#6105 = CARTESIAN_POINT ( 'NONE',  ( 2.826950749410920061, 20.19548487530456171, 2.214332391823603530 ) ) ;
#6106 = ORIENTED_EDGE ( 'NONE', *, *, #6925, .T. ) ;
#6107 = SURFACE_STYLE_USAGE ( .BOTH. , #5992 ) ;
#6108 = CIRCLE ( 'NONE', #9990, 1.983740000000001391 ) ;
#6109 = CARTESIAN_POINT ( 'NONE',  ( 6.177452850684594488, 20.35534769734861271, 5.182961054158671033 ) ) ;
#6110 = EDGE_CURVE ( 'NONE', #4736, #7142, #18741, .T. ) ;
#6111 = EDGE_CURVE ( 'NONE', #15942, #16009, #21617, .T. ) ;
#6112 = DIRECTION ( 'NONE',  ( 0.4987171968201936645, 0.000000000000000000, -0.8667647648559603235 ) ) ;
#6113 = CIRCLE ( 'NONE', #21664, 15.47812499999999680 ) ;
#6114 = VECTOR ( 'NONE', #19144, 1000.000000000000000 ) ;
#6115 = CARTESIAN_POINT ( 'NONE',  ( 7.235976006262752946, 20.89828364148222306, 1.503125890472612358 ) ) ;
#6116 = CARTESIAN_POINT ( 'NONE',  ( 5.363225780242031782, 15.84434817051344169, 8.012013768214686138 ) ) ;
#6117 = DIRECTION ( 'NONE',  ( 0.9579671649362033747, 0.000000000000000000, -0.2868778675745010664 ) ) ;
#6118 = CARTESIAN_POINT ( 'NONE',  ( 6.674888723083876485, 11.58565265486105211, 2.754745497594413450 ) ) ;
#6119 = DIRECTION ( 'NONE',  ( 0.9488823340533348860, -0.2002559181062069926, 0.2439669719141008553 ) ) ;
#6120 = DIRECTION ( 'NONE',  ( 0.2490110332224850509, 0.000000000000000000, -0.9685006480810792739 ) ) ;
#6121 = AXIS2_PLACEMENT_3D ( 'NONE', #14763, #21469, #19922 ) ;
#6122 = LINE ( 'NONE', #13324, #20122 ) ;
#6123 = VERTEX_POINT ( 'NONE', #16546 ) ;
#6124 = CARTESIAN_POINT ( 'NONE',  ( 17.79723720954694954, -1.983739999999999393, -14.07647485258271303 ) ) ;
#6125 = EDGE_CURVE ( 'NONE', #10206, #20031, #15597, .T. ) ;
#6126 = CARTESIAN_POINT ( 'NONE',  ( -47.86112874365709047, -5.714999999999999858, -23.29368419115692035 ) ) ;
#6127 = ORIENTED_EDGE ( 'NONE', *, *, #15590, .T. ) ;
#6128 = CARTESIAN_POINT ( 'NONE',  ( 9.405185730933931509, 17.20066956042925455, -2.794330434878057101 ) ) ;
#6129 = DIRECTION ( 'NONE',  ( 0.2490110332224857170, 0.000000000000000000, -0.9685006480810790519 ) ) ;
#6130 = VECTOR ( 'NONE', #17318, 1000.000000000000000 ) ;
#6131 = CARTESIAN_POINT ( 'NONE',  ( 0.7938407936894211758, 19.25142560623917376, 7.620760418591133067 ) ) ;
#6132 = CARTESIAN_POINT ( 'NONE',  ( 11.46521635664263172, -6.403241846889555333, -17.09334367148784750 ) ) ;
#6134 = LINE ( 'NONE', #4483, #11649 ) ;
#6133 = CARTESIAN_POINT ( 'NONE',  ( 5.870371952983467700, 11.25617621838232196, 2.534352863508499087 ) ) ;
#6135 = ORIENTED_EDGE ( 'NONE', *, *, #13900, .T. ) ;
#6136 =( NAMED_UNIT ( * ) SI_UNIT ( $, .STERADIAN. ) SOLID_ANGLE_UNIT ( ) );
#6137 = CARTESIAN_POINT ( 'NONE',  ( 16.85197508397059707, 13.08957250000000094, -16.77951971243562923 ) ) ;
#6138 = CARTESIAN_POINT ( 'NONE',  ( 30.33489826846160398, 32.54502000000000095, -2.417033907079745525 ) ) ;
#6139 = ORIENTED_EDGE ( 'NONE', *, *, #7483, .F. ) ;
#6140 = EDGE_CURVE ( 'NONE', #18115, #2722, #12408, .T. ) ;
#6141 = CARTESIAN_POINT ( 'NONE',  ( 20.17007366732797280, -1.298316440872414379, -14.77221745418293430 ) ) ;
#6142 = CARTESIAN_POINT ( 'NONE',  ( 0.3881773077461687649, 18.36706280121488533, 1.288916289607236365 ) ) ;
#6143 = VECTOR ( 'NONE', #10823, 1000.000000000000000 ) ;
#6144 = B_SPLINE_SURFACE_WITH_KNOTS ( 'NONE', 3, 3, ( 
 ( #132, #5432, #10308, #13532, #10423, #17050, #6657, #8414, #2004, #10525, #1897, #5319, #16833, #12087, #5002, #1674, #3566, #15418, #13753, #11758, #245, #10191, #17, #15191, #15309, #8743, #12197, #10088, #3456, #1578, #16935, #6983, #8319, #15524, #15090, #21803, #20239, #20343, #7101, #13417, #6767, #13643, #5211, #1784, #8529, #9303, #12747, #5659, #3901, #17395, #17500, #19360, #19027, #580, #12418, #8858, #682, #21124, #7427, #10642, #4339, #473, #4225, #2235, #7227, #8973, #14409 ),
 ( #17603, #14309, #15753, #5872, #20684, #7324, #12532, #2457, #7546, #13986, #9185, #4012, #14087, #20792, #9077, #12636, #5976, #19146, #10754, #19468, #2347, #10857, #17271, #4115, #2118, #7648, #15852, #15642, #14200, #20914, #5541, #5777, #19256, #15965, #799, #12299, #10965, #21026, #17717, #2568, #16077, #907, #11080, #1005, #4773, #14848, #14961, #2893, #8073, #11405, #21448, #6419, #21563, #11287, #14520, #7861, #13189, #6305, #21342, #16391, #11504, #19786, #19898, #6093, #7971, #6200, #19679 ),
 ( #16602, #16284, #2681, #8187, #13299, #1330, #13079, #12864, #7754, #17934, #21236, #3106, #4660, #18247, #16495, #9831, #11182, #4548, #18153, #21675, #1440, #4451, #19583, #12971, #9627, #6537, #3006, #18037, #1228, #20001, #9733, #17835, #2779, #14742, #9411, #16179, #9514, #1118, #14638, #21781, #13619, #1758, #18465, #4871, #15283, #15394, #10167, #8502, #11839, #3332, #17024, #327, #10396, #17140, #13837, #20103, #18350, #108, #15499, #219, #20421, #18568, #6629, #15165, #16911, #6858, #4973 ),
 ( #20318, #11730, #9952, #18782, #7071, #11957, #10063, #16811, #5091, #6959, #1651, #8392, #6742, #3215, #5188, #8723, #11939, #13506, #11615, #16713, #5289, #20218, #1551, #3432, #1982, #18668, #15066, #3539, #10275, #1872, #12055, #8294, #8617, #3652, #17687, #5748, #17576, #10828, #10727, #20878, #14173, #550, #17469, #15826, #18894, #9049, #12504, #2538, #2315, #9271, #14061, #15607, #19000, #7297, #8831, #20999, #12170, #653, #17247, #16047, #878, #19329, #8947, #5629, #20543, #9155, #2430 ),
 ( #19226, #19115, #5406, #12390, #4087, #4194, #15938, #444, #12603, #766, #7517, #14282, #3765, #7197, #20767, #13957, #20655, #15724, #3984, #10502, #5516, #12275, #3876, #17363, #2205, #13775, #3480, #44, #8884, #12321, #5232, #10217, #16964, #17078, #18939, #18614, #159, #18723, #8444, #266, #20709, #7008, #1813, #3925, #6797, #3811, #8557, #13557, #15334, #14007, #11886, #5134, #12111, #3593, #6902, #10546, #15215, #2023, #13666, #5564, #8766, #13899, #7130, #20478, #15548, #3704, #10334 ),
 ( #20367, #1921, #19048, #8666, #10445, #16858, #379, #1703, #7248, #15438, #20262, #5348, #18836, #20598, #5456, #12220, #17294, #2141, #15666, #495, #17522, #15878, #14431, #927, #9431, #8996, #600, #16203, #15774, #14223, #12656, #7671, #20942, #17628, #21700, #1462, #4685, #7885, #1250, #8210, #14869, #14764, #9752, #20021, #13211, #4890, #21366, #1347, #21470, #13101, #6222, #16308, #9851, #12993, #19923, #8091, #18062, #4469, #21586, #14985, #16515, #6446, #11429, #2921, #16620, #21799, #9977 ),
 ( #19812, #4796, #1575, #6555, #16735, #8316, #11205, #15087, #11634, #19699, #7990, #18371, #4573, #6327, #6653, #16419, #11313, #17955, #2803, #9538, #18175, #3240, #3029, #1143, #11528, #18269, #14660, #3127, #9650, #5111, #7098, #469, #20446, #17161, #13528, #8740, #1671, #20235, #15414, #5316, #10420, #16830, #12080, #6880, #18586, #11859, #11963, #15520, #8855, #6764, #1781, #15638, #13640, #13749, #7222, #6980, #2114, #10521, #10187, #20124, #18693, #17047, #18484, #3561, #8524, #16930, #3453 ),
 ( #15305, #2000, #18807, #349, #4997, #10085, #13866, #20568, #11753, #10303, #5429, #3676, #8641, #12194, #18916, #20340, #8409, #129, #3786, #242, #5208, #1894, #17267, #3357, #15187, #14, #10851, #9074, #678, #15748, #3897, #19354, #8970, #795, #17600, #5654, #13983, #9182, #2565, #19253, #15962, #20911, #12415, #4221, #9407, #19465, #4336, #1002, #577, #5538, #7542, #2678, #9299, #7645, #5773, #14084, #2341, #4112, #14306, #20789, #20680, #5869, #12529, #19143, #15849, #21023, #12633 ),
 ( #10961, #17714, #4008, #19022, #5970, #16176, #7423, #10752, #17497, #14196, #16074, #904, #14406, #21121, #12296, #12743, #17831, #11076, #10639, #17391, #2231, #9827, #14634, #19580, #21339, #4867, #2776, #17931, #3002, #18032, #1113, #16596, #6090, #8068, #19676, #11611, #14844, #4767, #19894, #19782, #21559, #16490, #9621, #4656, #9729, #12860, #18147, #6415, #18344, #11401, #3210, #1224, #9511, #6197, #16387, #11178, #8183, #21233, #1326, #4447, #19996, #9948, #6533, #2889, #14737, #7751, #18243 ) ),
 .UNSPECIFIED., .F., .F., .F.,
 ( 4, 1, 1, 1, 1, 1, 4 ),
 ( 4, 1, 1, 1, 1, 1, 1, 1, 1, 1, 1, 1, 1, 1, 1, 1, 1, 1, 1, 1, 1, 1, 1, 1, 1, 1, 1, 1, 1, 1, 1, 1, 1, 1, 1, 1, 1, 1, 1, 1, 1, 1, 1, 1, 1, 1, 1, 1, 1, 1, 1, 1, 1, 1, 1, 1, 1, 1, 1, 1, 1, 1, 1, 1, 4 ),
 ( -0.01121212662510000062, 0.000000000000000000, 0.1250000000000000000, 0.2500000000000000000, 0.3750000000000000000, 0.5000000000000000000, 0.5112121266250999607 ),
 ( -0.02000000000000000042, -0.003749999999999999861, 0.01250000000000000069, 0.02875000000000000125, 0.04499999999999999833, 0.06124999999999999889, 0.07749999999999999944, 0.09375000000000000000, 0.1100000000000000006, 0.1262500000000000011, 0.1424999999999999878, 0.1587500000000000022, 0.1749999999999999889, 0.1912500000000000033, 0.2074999999999999900, 0.2237500000000000044, 0.2399999999999999911, 0.2562499999999999778, 0.2725000000000000200, 0.2887500000000000067, 0.3049999999999999933, 0.3212499999999999800, 0.3375000000000000222, 0.3537500000000000089, 0.3699999999999999956, 0.3862499999999999822, 0.4025000000000000244, 0.4187500000000000111, 0.4349999999999999978, 0.4512499999999999845, 0.4675000000000000266, 0.4837500000000000133, 0.5000000000000000000, 0.5162499999999999867, 0.5324999999999999734, 0.5487499999999999600, 0.5649999999999999467, 0.5812500000000000444, 0.5975000000000000311, 0.6137500000000000178, 0.6300000000000000044, 0.6462499999999999911, 0.6624999999999999778, 0.6787499999999999645, 0.6949999999999999512, 0.7112500000000000488, 0.7275000000000000355, 0.7437500000000000222, 0.7600000000000000089, 0.7762499999999999956, 0.7924999999999999822, 0.8087499999999999689, 0.8249999999999999556, 0.8412500000000000533, 0.8575000000000000400, 0.8737500000000000266, 0.8900000000000000133, 0.9062500000000000000, 0.9224999999999999867, 0.9387499999999999734, 0.9549999999999999600, 0.9712499999999999467, 0.9875000000000000444, 1.003749999999999920, 1.020000000000000018 ),
 .UNSPECIFIED. ) ;
#6145 = EDGE_LOOP ( 'NONE', ( #13443, #13119, #314, #6996 ) ) ;
#6146 = CARTESIAN_POINT ( 'NONE',  ( 13.16968626221765248, 14.87475635823169640, 6.322754070328278075 ) ) ;
#6147 = DIRECTION ( 'NONE',  ( -0.9685006480810792739, 0.000000000000000000, -0.2490110332224846346 ) ) ;
#6148 = CARTESIAN_POINT ( 'NONE',  ( 6.861624739425660202, 21.59165172380602371, 1.401955922046088210 ) ) ;
#6149 = CIRCLE ( 'NONE', #16752, 0.5079999999999984528 ) ;
#6150 = CARTESIAN_POINT ( 'NONE',  ( 20.05951646036145064, -3.617492969892214916, -15.31622960476870077 ) ) ;
#6151 = CARTESIAN_POINT ( 'NONE',  ( 38.95866807045890567, -7.547549837578408471, -3.945694591016585928 ) ) ;
#6152 = EDGE_LOOP ( 'NONE', ( #5506, #18102, #17963, #9276 ) ) ;
#6153 = FACE_OUTER_BOUND ( 'NONE', #8027, .T. ) ;
#6154 = ADVANCED_FACE ( 'NONE', ( #1379 ), #10266, .T. ) ;
#6155 = DIRECTION ( 'NONE',  ( -0.08192867786951699149, 0.000000000000000000, -0.9966381950048638361 ) ) ;
#6156 = VECTOR ( 'NONE', #16143, 1000.000000000000114 ) ;
#6157 = ORIENTED_EDGE ( 'NONE', *, *, #11852, .T. ) ;
#6158 = EDGE_CURVE ( 'NONE', #8937, #11827, #8240, .T. ) ;
#6159 = EDGE_LOOP ( 'NONE', ( #14102, #19969, #4301, #8895 ) ) ;
#6160 = EDGE_CURVE ( 'NONE', #17319, #8651, #4825, .T. ) ;
#6161 = CARTESIAN_POINT ( 'NONE',  ( 11.62103910360368353, -6.985094744456809224, -15.76249710157855155 ) ) ;
#6163 = DIRECTION ( 'NONE',  ( -0.9964481331860212121, 0.000000000000000000, 0.08420877549337303647 ) ) ;
#6162 = CARTESIAN_POINT ( 'NONE',  ( 0.2333143917931327360, 19.02276410538376084, 0.6558456349049158751 ) ) ;
#6164 = VERTEX_POINT ( 'NONE', #6358 ) ;
#6165 = CARTESIAN_POINT ( 'NONE',  ( 3.524832663404014355, 15.96368446185943135, -1.413071295161979712 ) ) ;
#6166 = ORIENTED_EDGE ( 'NONE', *, *, #17405, .F. ) ;
#6167 = VERTEX_POINT ( 'NONE', #21619 ) ;
#6168 = AXIS2_PLACEMENT_3D ( 'NONE', #923, #2914, #21141 ) ;
#6169 = CARTESIAN_POINT ( 'NONE',  ( 1.076515439104938299, 12.50515649462741763, 6.318341509549295409 ) ) ;
#6170 = ORIENTED_EDGE ( 'NONE', *, *, #12226, .T. ) ;
#6171 = AXIS2_PLACEMENT_3D ( 'NONE', #5624, #7397, #20874 ) ;
#6172 = CARTESIAN_POINT ( 'NONE',  ( 12.59675778470975516, -14.84248999999999974, -12.54640024901842033 ) ) ;
#6173 = DIRECTION ( 'NONE',  ( 0.000000000000000000, 1.000000000000000000, 0.000000000000000000 ) ) ;
#6174 = FACE_OUTER_BOUND ( 'NONE', #11039, .T. ) ;
#6175 = DIRECTION ( 'NONE',  ( 1.000000000000000000, 0.000000000000000000, 0.000000000000000000 ) ) ;
#6176 = CARTESIAN_POINT ( 'NONE',  ( 3.518193601275699578, 13.18433185408993147, 8.140409692525564012 ) ) ;
#6177 = ORIENTED_EDGE ( 'NONE', *, *, #4747, .F. ) ;
#6178 = CARTESIAN_POINT ( 'NONE',  ( 28.87608719841374949, 40.07707250000000698, -15.73691681567849976 ) ) ;
#6179 = DIRECTION ( 'NONE',  ( 0.9685006480810791629, 0.000000000000000000, 0.2490110332224850231 ) ) ;
#6180 = DIRECTION ( 'NONE',  ( 0.000000000000000000, -1.000000000000000000, 0.000000000000000000 ) ) ;
#6181 = CARTESIAN_POINT ( 'NONE',  ( 47.80475250345343596, 38.88803500000000213, -11.91473563638196786 ) ) ;
#6182 = VERTEX_POINT ( 'NONE', #21832 ) ;
#6183 = EDGE_CURVE ( 'NONE', #3518, #20164, #8343, .T. ) ;
#6184 = ORIENTED_EDGE ( 'NONE', *, *, #21665, .F. ) ;
#6185 = CARTESIAN_POINT ( 'NONE',  ( 5.496113507260316666, 12.63305981940006184, 0.2285824550650361886 ) ) ;
#6187 = CARTESIAN_POINT ( 'NONE',  ( -22.72495373119935635, -0.3962399999999990929, 1.006347609994784120 ) ) ;
#6186 = DIRECTION ( 'NONE',  ( 0.2490110332224846623, 0.000000000000000000, -0.9685006480810793850 ) ) ;
#6188 = CARTESIAN_POINT ( 'NONE',  ( 12.00464716003233434, 21.22932480519864029, -1.908312899720273181 ) ) ;
#6189 = ORIENTED_EDGE ( 'NONE', *, *, #319, .T. ) ;
#6190 = AXIS2_PLACEMENT_3D ( 'NONE', #5257, #4848, #21752 ) ;
#6191 = ORIENTED_EDGE ( 'NONE', *, *, #12203, .T. ) ;
#6192 = FACE_OUTER_BOUND ( 'NONE', #3880, .T. ) ;
#6193 = CARTESIAN_POINT ( 'NONE',  ( 8.499614257248339300, 21.33403448576225259, 0.06076556050593111269 ) ) ;
#6194 = CARTESIAN_POINT ( 'NONE',  ( 9.061696275389516941, 17.79575755247912738, 7.005266136422250156 ) ) ;
#6195 = CARTESIAN_POINT ( 'NONE',  ( 13.72479379337794825, 21.95613576153688484, 1.820250569444666233 ) ) ;
#6196 = CARTESIAN_POINT ( 'NONE',  ( -17.46249999999999858, 32.54502000000000095, 0.000000000000000000 ) ) ;
#6197 = CARTESIAN_POINT ( 'NONE',  ( 4.362043098078323133, 20.54185615358932182, 0.4015571536017943366 ) ) ;
#6198 = CARTESIAN_POINT ( 'NONE',  ( 1.268452225264728561, 11.99997494541211651, 7.084638612796553936 ) ) ;
#6199 = VERTEX_POINT ( 'NONE', #9883 ) ;
#6200 = CARTESIAN_POINT ( 'NONE',  ( 6.062088034068962017, 12.01182390341870310, 1.443241840189279701 ) ) ;
#6201 = CARTESIAN_POINT ( 'NONE',  ( 26.59062499999999929, 26.59189500000000095, 8.731249999999999289 ) ) ;
#6202 = DIRECTION ( 'NONE',  ( 0.000000000000000000, -1.000000000000000000, 0.000000000000000000 ) ) ;
#6203 = CARTESIAN_POINT ( 'NONE',  ( 11.22892694877909037, -5.901286635516172829, -15.87608302377674363 ) ) ;
#6204 = VERTEX_POINT ( 'NONE', #16648 ) ;
#6205 = CARTESIAN_POINT ( 'NONE',  ( 49.72033008250774344, -1.983739999999999837, -2.687827786179598277 ) ) ;
#6206 = EDGE_CURVE ( 'NONE', #15542, #11564, #21729, .T. ) ;
#6207 = CARTESIAN_POINT ( 'NONE',  ( 9.070049129643198427, 15.38332000535482180, -3.534303114342071783 ) ) ;
#6208 = VERTEX_POINT ( 'NONE', #3275 ) ;
#6209 = LINE ( 'NONE', #9311, #11351 ) ;
#6210 = CARTESIAN_POINT ( 'NONE',  ( 11.88511336867002299, 20.02872603525521455, -2.122466797632162283 ) ) ;
#6211 = CARTESIAN_POINT ( 'NONE',  ( 6.300610883601452272, 20.63257317582153405, -0.1521459510048163710 ) ) ;
#6212 = FACE_OUTER_BOUND ( 'NONE', #5840, .T. ) ;
#6213 = CARTESIAN_POINT ( 'NONE',  ( -0.7853767243149117894, 19.84627995571224091, 3.566713853412147195 ) ) ;
#6214 = EDGE_LOOP ( 'NONE', ( #1917, #16429, #16272, #7308, #2969 ) ) ;
#6215 = CARTESIAN_POINT ( 'NONE',  ( 23.49608546833631451, 28.96330250000000461, -17.12016812500874252 ) ) ;
#6216 = APPLICATION_CONTEXT ( 'automotive_design' ) ;
#6217 = DIRECTION ( 'NONE',  ( -0.000000000000000000, -1.000000000000000000, 0.000000000000000000 ) ) ;
#6218 = EDGE_LOOP ( 'NONE', ( #15211, #20520, #2063, #9799, #9801 ) ) ;
#6219 = CARTESIAN_POINT ( 'NONE',  ( 44.27024749654656688, -7.547609999999999708, -8.722764363618033201 ) ) ;
#6220 = CARTESIAN_POINT ( 'NONE',  ( 11.08655503941167808, 19.16255833366876260, 6.076062753481236811 ) ) ;
#6221 = DIRECTION ( 'NONE',  ( -0.2868778675745008999, 0.000000000000000000, -0.9579671649362034858 ) ) ;
#6222 = CARTESIAN_POINT ( 'NONE',  ( 3.804155136816291805, 15.46201706931346465, -1.459015595820115196 ) ) ;
#6223 = DIRECTION ( 'NONE',  ( -0.8609107660235849613, 0.000000000000000000, 0.5087559856598092844 ) ) ;
#6224 = DIRECTION ( 'NONE',  ( -0.9724402360367336851, 0.000000000000000000, 0.2331522835762537549 ) ) ;
#6225 = CARTESIAN_POINT ( 'NONE',  ( 6.537126953640395755, 11.68813007582838281, 2.803481180618996316 ) ) ;
#6226 = LINE ( 'NONE', #21370, #10438 ) ;
#6227 = CARTESIAN_POINT ( 'NONE',  ( 20.35347976045076734, -6.056219266232003129, -15.15089302274523497 ) ) ;
#6228 = CARTESIAN_POINT ( 'NONE',  ( 64.19677489640052670, 34.52875999999999834, -11.74367670905533423 ) ) ;
#6229 = ADVANCED_FACE ( 'NONE', ( #10009 ), #1913, .F. ) ;
#6230 = ORIENTED_EDGE ( 'NONE', *, *, #11251, .T. ) ;
#6231 = DIRECTION ( 'NONE',  ( 0.6496772031432432870, 0.000000000000000000, -0.7602101891687411683 ) ) ;
#6232 = DIRECTION ( 'NONE',  ( 0.9685006480810790519, 0.000000000000000000, 0.2490110332224857170 ) ) ;
#6233 = ORIENTED_EDGE ( 'NONE', *, *, #9501, .T. ) ;
#6234 = CARTESIAN_POINT ( 'NONE',  ( 10.10020702742011345, 20.09850238419586788, -1.233466479950767747 ) ) ;
#6235 = CARTESIAN_POINT ( 'NONE',  ( 44.27024749654656688, 40.07865999999999929, -8.722764363618033201 ) ) ;
#6236 = CIRCLE ( 'NONE', #239, 3.175000000000000711 ) ;
#6237 = CARTESIAN_POINT ( 'NONE',  ( 1.089698143903370164, 18.39942038070247676, 8.297769702651454082 ) ) ;
#6238 = CARTESIAN_POINT ( 'NONE',  ( 23.41562500000000213, 32.54502000000000095, 5.159374999999999822 ) ) ;
#6239 = EDGE_LOOP ( 'NONE', ( #18212, #12455, #9928, #6494 ) ) ;
#6240 =( LENGTH_UNIT ( ) NAMED_UNIT ( * ) SI_UNIT ( .MILLI., .METRE. ) );
#6241 = DIRECTION ( 'NONE',  ( 0.000000000000000000, -1.000000000000000000, 0.000000000000000000 ) ) ;
#6242 = DIRECTION ( 'NONE',  ( 0.000000000000000000, 1.000000000000000000, 0.000000000000000000 ) ) ;
#6243 = ORIENTED_EDGE ( 'NONE', *, *, #149, .F. ) ;
#6244 = LINE ( 'NONE', #6352, #10771 ) ;
#6245 = CARTESIAN_POINT ( 'NONE',  ( 14.87174356566636035, -8.043846378258365348, -15.78031415564158735 ) ) ;
#6246 = ORIENTED_EDGE ( 'NONE', *, *, #15458, .T. ) ;
#6247 = CARTESIAN_POINT ( 'NONE',  ( 7.626071724256386020, 18.07321731131985842, -1.931034283370769877 ) ) ;
#6248 = EDGE_CURVE ( 'NONE', #2429, #12596, #2159, .T. ) ;
#6249 = CARTESIAN_POINT ( 'NONE',  ( 38.76233322772463197, 40.04759419886305949, -4.169083009079019853 ) ) ;
#6250 = CARTESIAN_POINT ( 'NONE',  ( 8.404128694230886154, 21.35170238401046205, -0.1542871241044822539 ) ) ;
#6251 = CARTESIAN_POINT ( 'NONE',  ( 19.92745932268303477, -1.805445330691633155, -15.43621892734358525 ) ) ;
#6252 = FACE_OUTER_BOUND ( 'NONE', #21429, .T. ) ;
#6253 = EDGE_CURVE ( 'NONE', #9783, #8950, #18714, .T. ) ;
#6254 = ORIENTED_EDGE ( 'NONE', *, *, #5578, .F. ) ;
#6255 = EDGE_CURVE ( 'NONE', #21636, #8132, #2844, .T. ) ;
#6256 = ADVANCED_FACE ( 'NONE', ( #16639 ), #16754, .T. ) ;
#6257 = DIRECTION ( 'NONE',  ( 0.9685006480810793850, 0.000000000000000000, 0.2490110332224849121 ) ) ;
#6258 = CARTESIAN_POINT ( 'NONE',  ( 30.50878709810603340, -4.569743463999999200, -19.83971405306587954 ) ) ;
#6259 = VERTEX_POINT ( 'NONE', #10322 ) ;
#6260 = ORIENTED_EDGE ( 'NONE', *, *, #4201, .T. ) ;
#6261 = PLANE ( 'NONE',  #21860 ) ;
#6263 = CARTESIAN_POINT ( 'NONE',  ( 46.03750000000000142, 0.000000000000000000, -10.31874999999999964 ) ) ;
#6262 = CARTESIAN_POINT ( 'NONE',  ( 5.488110206262358126, 13.84264232191805100, 8.338955251487456977 ) ) ;
#6264 = EDGE_LOOP ( 'NONE', ( #14536, #11321, #2359, #2878, #7202, #6870, #531, #8223, #12958, #10461, #14034, #189, #1680, #3502, #19195, #11540, #16282, #297, #6592, #4059, #2387, #11791, #16453, #11632, #21217, #19822, #7471, #21064, #9039, #3214, #15807, #4728, #5187, #2527, #9558, #3862, #6288, #41, #4659, #19587 ) ) ;
#6265 = CARTESIAN_POINT ( 'NONE',  ( 4.408559984239932561, 20.45280785655899436, 0.4597285100094092303 ) ) ;
#6266 = ORIENTED_EDGE ( 'NONE', *, *, #18200, .F. ) ;
#6267 = CIRCLE ( 'NONE', #1667, 0.7950200000000000600 ) ;
#6268 = ORIENTED_EDGE ( 'NONE', *, *, #2393, .F. ) ;
#6269 = ORIENTED_EDGE ( 'NONE', *, *, #20987, .F. ) ;
#6270 = CARTESIAN_POINT ( 'NONE',  ( 2.316111848326288136, 12.35794879854923778, 2.694249400427293661 ) ) ;
#6271 = EDGE_CURVE ( 'NONE', #21107, #5161, #1692, .T. ) ;
#6272 = LINE ( 'NONE', #4416, #12078 ) ;
#6273 = CARTESIAN_POINT ( 'NONE',  ( 1.998220421679061776, -1.515722362770699494, -22.64748046904500356 ) ) ;
#6274 = DIRECTION ( 'NONE',  ( 0.000000000000000000, 0.000000000000000000, -1.000000000000000000 ) ) ;
#6275 = CARTESIAN_POINT ( 'NONE',  ( 2.228897815535521243, 11.62399859808463276, 2.403690802849292041 ) ) ;
#6276 = VECTOR ( 'NONE', #12521, 1000.000000000000000 ) ;
#6277 = ORIENTED_EDGE ( 'NONE', *, *, #10409, .T. ) ;
#6278 = EDGE_CURVE ( 'NONE', #11569, #19768, #10299, .T. ) ;
#6279 = LINE ( 'NONE', #18006, #12839 ) ;
#6280 = CARTESIAN_POINT ( 'NONE',  ( 26.59062499999999929, 2.380615000000000148, 8.731249999999999289 ) ) ;
#6281 = LINE ( 'NONE', #1205, #4965 ) ;
#6282 = DIRECTION ( 'NONE',  ( 0.08420877549337302259, 0.000000000000000000, 0.9964481331860212121 ) ) ;
#6283 = EDGE_LOOP ( 'NONE', ( #16160, #7434, #12663, #4123 ) ) ;
#6284 = ORIENTED_EDGE ( 'NONE', *, *, #16958, .F. ) ;
#6285 = CARTESIAN_POINT ( 'NONE',  ( 8.738383752483903422, 18.26872045576617865, 7.110093598169133777 ) ) ;
#6286 = CARTESIAN_POINT ( 'NONE',  ( 41.71184157647478230, 38.88803500000000213, -2.134205101306931862 ) ) ;
#6287 = CARTESIAN_POINT ( 'NONE',  ( 10.96708857545880278, 16.60965070755050732, -4.348602899851927717 ) ) ;
#6288 = ORIENTED_EDGE ( 'NONE', *, *, #11325, .T. ) ;
#6289 = ORIENTED_EDGE ( 'NONE', *, *, #21665, .T. ) ;
#6290 = DIRECTION ( 'NONE',  ( 0.000000000000000000, 1.000000000000000000, 0.000000000000000000 ) ) ;
#6291 = CARTESIAN_POINT ( 'NONE',  ( 8.327267709314158495, 20.16378942260824303, 5.275824550407316238 ) ) ;
#6292 = VECTOR ( 'NONE', #6349, 1000.000000000000114 ) ;
#6293 = CARTESIAN_POINT ( 'NONE',  ( 3.191353643069211543, 17.79477638262715189, 8.193924954953159201 ) ) ;
#6294 = EDGE_CURVE ( 'NONE', #9547, #8281, #15206, .T. ) ;
#6295 = ADVANCED_FACE ( 'NONE', ( #11550 ), #1482, .T. ) ;
#6296 = CARTESIAN_POINT ( 'NONE',  ( 31.83819605565793509, -3.968114999999999615, -4.158220719828246814 ) ) ;
#6297 = AXIS2_PLACEMENT_3D ( 'NONE', #3263, #21820, #4708 ) ;
#6298 = CARTESIAN_POINT ( 'NONE',  ( 13.48553132191480763, 22.15489287403912400, 1.921071336905035842 ) ) ;
#6299 = DIRECTION ( 'NONE',  ( 0.000000000000000000, 0.000000000000000000, 1.000000000000000000 ) ) ;
#6300 = CYLINDRICAL_SURFACE ( 'NONE', #20814, 0.5079999999999996740 ) ;
#6301 = DIRECTION ( 'NONE',  ( -0.1132953773954069598, 0.7241889112991808375, -0.6802312681817410667 ) ) ;
#6302 = CARTESIAN_POINT ( 'NONE',  ( 1.593482295714299557, 17.10159210520789586, 9.552994227452236586 ) ) ;
#6303 = FACE_OUTER_BOUND ( 'NONE', #21330, .T. ) ;
#6304 = EDGE_LOOP ( 'NONE', ( #3709, #2071, #18573, #7081 ) ) ;
#6305 = CARTESIAN_POINT ( 'NONE',  ( 6.667155597571054138, 19.52118532600693968, 6.488507913781226044 ) ) ;
#6306 = DIRECTION ( 'NONE',  ( 0.2868778675745011220, 0.000000000000000000, 0.9579671649362034858 ) ) ;
#6307 = CARTESIAN_POINT ( 'NONE',  ( 50.62387473582167274, -1.983739999999999837, -28.41576006634952734 ) ) ;
#6308 = CARTESIAN_POINT ( 'NONE',  ( 10.94429949547802217, -5.371352442010961958, -15.92721155031827429 ) ) ;
#6309 = DIRECTION ( 'NONE',  ( 0.4987171968201928873, 0.000000000000000000, -0.8667647648559606566 ) ) ;
#6310 = VERTEX_POINT ( 'NONE', #20255 ) ;
#6311 = CARTESIAN_POINT ( 'NONE',  ( 55.33978576324753362, 0.000000000000000000, -23.05096232720518756 ) ) ;
#6312 = CARTESIAN_POINT ( 'NONE',  ( 11.23181352795878141, 22.17023050789328309, 2.056103838605086498 ) ) ;
#6313 = CIRCLE ( 'NONE', #14106, 9.525000000000002132 ) ;
#6314 = CARTESIAN_POINT ( 'NONE',  ( 9.164819943473123232, 13.37848835739949038, -2.805861135747332202 ) ) ;
#6315 = ORIENTED_EDGE ( 'NONE', *, *, #1935, .F. ) ;
#6316 = CARTESIAN_POINT ( 'NONE',  ( 26.66313208013160008, 1.184654662339226006, 10.54777226219331965 ) ) ;
#6317 = CARTESIAN_POINT ( 'NONE',  ( 8.699141033147567370, 20.29604414026289660, 6.341648953013584666 ) ) ;
#6318 = CYLINDRICAL_SURFACE ( 'NONE', #12698, 9.524999999999998579 ) ;
#6319 = CARTESIAN_POINT ( 'NONE',  ( 2.391745392645233892, 20.09535866699502193, 6.285321213869885071 ) ) ;
#6320 = DIRECTION ( 'NONE',  ( -0.2672484743474505819, 0.000000000000000000, -0.9636276526537416176 ) ) ;
#6321 = DIRECTION ( 'NONE',  ( -0.000000000000000000, -1.000000000000000000, 0.000000000000000000 ) ) ;
#6322 = ADVANCED_FACE ( 'NONE', ( #4908 ), #9872, .F. ) ;
#6323 = VECTOR ( 'NONE', #10556, 1000.000000000000000 ) ;
#6324 = CARTESIAN_POINT ( 'NONE',  ( 0.05261182704408059324, 23.41816500000000190, 7.316601101023040066 ) ) ;
#6325 = CARTESIAN_POINT ( 'NONE',  ( 12.78645908641997941, 20.00510796315846207, 5.045423586650715109 ) ) ;
#6326 = LINE ( 'NONE', #16418, #18686 ) ;
#6327 = CARTESIAN_POINT ( 'NONE',  ( 0.1330856713724426765, 12.52330284320706077, 1.635176554771325064 ) ) ;
#6328 = CARTESIAN_POINT ( 'NONE',  ( -1.345424459097947834, 20.24316500000000119, 2.648158502653860324 ) ) ;
#6329 = VECTOR ( 'NONE', #16215, 1000.000000000000114 ) ;
#6330 = FACE_OUTER_BOUND ( 'NONE', #17771, .T. ) ;
#6331 = CARTESIAN_POINT ( 'NONE',  ( 6.768681381451962409, 11.33814276891691186, 2.708583584588580173 ) ) ;
#6332 = DIRECTION ( 'NONE',  ( -0.7421532822901579785, 0.000000000000000000, 0.6702301885068630005 ) ) ;
#6333 = CARTESIAN_POINT ( 'NONE',  ( 20.08791609653252053, -6.411858537233912969, -15.20285343563792679 ) ) ;
#6334 = DIRECTION ( 'NONE',  ( 0.000000000000000000, 1.000000000000000000, 0.000000000000000000 ) ) ;
#6335 = ORIENTED_EDGE ( 'NONE', *, *, #3459, .T. ) ;
#6336 = FACE_OUTER_BOUND ( 'NONE', #7758, .T. ) ;
#6337 = CARTESIAN_POINT ( 'NONE',  ( 10.91631540834134206, 12.36537083236676082, 4.900493360693962686 ) ) ;
#6338 = CARTESIAN_POINT ( 'NONE',  ( 53.69636427252483202, 38.88803500000000213, -18.48840734645144224 ) ) ;
#6339 = ORIENTED_EDGE ( 'NONE', *, *, #4097, .F. ) ;
#6340 = CARTESIAN_POINT ( 'NONE',  ( 9.740401853436322810, 19.04328518575157858, -2.119098382970255656 ) ) ;
#6341 = CARTESIAN_POINT ( 'NONE',  ( 22.02657784715807665, -3.968114999999999615, -12.98906981665815330 ) ) ;
#6342 = CARTESIAN_POINT ( 'NONE',  ( 52.22364792556211910, 38.56942770589630953, -17.56175453227104200 ) ) ;
#6343 = CARTESIAN_POINT ( 'NONE',  ( 14.68672346071107171, -7.556859706525174580, -14.66503917285335845 ) ) ;
#6345 = CARTESIAN_POINT ( 'NONE',  ( 38.60701496492545459, 32.54502000000000095, -26.94161103631838472 ) ) ;
#6344 = CARTESIAN_POINT ( 'NONE',  ( 1.095999888774144893, 17.17955240639085801, 9.025385985431823244 ) ) ;
#6346 = ORIENTED_EDGE ( 'NONE', *, *, #6413, .T. ) ;
#6347 = CARTESIAN_POINT ( 'NONE',  ( 28.56548256563643662, -3.968114999999999615, -12.12873025803960658 ) ) ;
#6348 = CARTESIAN_POINT ( 'NONE',  ( 3.733612400581542090, 15.38343507826679257, -0.5588609866527980419 ) ) ;
#6349 = DIRECTION ( 'NONE',  ( -0.8609107660235849613, 0.000000000000000000, 0.5087559856598092844 ) ) ;
#6350 = ORIENTED_EDGE ( 'NONE', *, *, #14654, .F. ) ;
#6351 = CIRCLE ( 'NONE', #21878, 0.7950200000000005041 ) ;
#6352 = CARTESIAN_POINT ( 'NONE',  ( 29.22749461619170219, 39.28268749999999443, -4.986088976786413163 ) ) ;
#6353 = VECTOR ( 'NONE', #2772, 1000.000000000000114 ) ;
#6354 = EDGE_CURVE ( 'NONE', #490, #17754, #1804, .T. ) ;
#6355 = CARTESIAN_POINT ( 'NONE',  ( 21.12774895840593103, -3.365576380264218237, -15.73708478087671558 ) ) ;
#6356 = ORIENTED_EDGE ( 'NONE', *, *, #7613, .T. ) ;
#6357 = CARTESIAN_POINT ( 'NONE',  ( 6.090447438359761989, 11.87235548079908298, 1.620859727200755440 ) ) ;
#6358 = CARTESIAN_POINT ( 'NONE',  ( 2.063750000000000195, 24.21318500000000284, 10.71562499999999929 ) ) ;
#6359 = CARTESIAN_POINT ( 'NONE',  ( 9.503040939678710330, 14.64581734927065249, 7.855185963858965614 ) ) ;
#6360 = AXIS2_PLACEMENT_3D ( 'NONE', #1884, #7309, #8631 ) ;
#6361 = CARTESIAN_POINT ( 'NONE',  ( 42.27821610176829381, -1.983739999999999837, 7.496956594510385763 ) ) ;
#6362 = LINE ( 'NONE', #15672, #4249 ) ;
#6363 = EDGE_LOOP ( 'NONE', ( #7392, #13518, #4896, #17810 ) ) ;
#6364 = CIRCLE ( 'NONE', #6713, 0.7950200000000000600 ) ;
#6365 = DIRECTION ( 'NONE',  ( -0.000000000000000000, -1.000000000000000000, 0.000000000000000000 ) ) ;
#6366 = VECTOR ( 'NONE', #1282, 1000.000000000000114 ) ;
#6367 = DIRECTION ( 'NONE',  ( -0.9685006480810793850, 0.000000000000000000, -0.2490110332224846623 ) ) ;
#6368 = ORIENTED_EDGE ( 'NONE', *, *, #18799, .F. ) ;
#6369 = EDGE_LOOP ( 'NONE', ( #17817, #7925, #16660, #13328 ) ) ;
#6370 = CARTESIAN_POINT ( 'NONE',  ( 20.05229758337772594, 0.5585561380493306860, -14.21405859630069912 ) ) ;
#6372 = CARTESIAN_POINT ( 'NONE',  ( 37.51913901087312553, 42.06303499999999929, -14.58057485080488114 ) ) ;
#6371 = CARTESIAN_POINT ( 'NONE',  ( 1.638698297806659543, 15.58835493759099400, 9.687949104223214647 ) ) ;
#6373 = VERTEX_POINT ( 'NONE', #18391 ) ;
#6374 = CARTESIAN_POINT ( 'NONE',  ( 3.511412721642198420, 15.31161194722795216, -1.319329340395489325 ) ) ;
#6375 = EDGE_CURVE ( 'NONE', #8773, #3294, #6895, .T. ) ;
#6376 = ORIENTED_EDGE ( 'NONE', *, *, #19723, .F. ) ;
#6377 = VECTOR ( 'NONE', #13383, 1000.000000000000114 ) ;
#6378 = VERTEX_POINT ( 'NONE', #1595 ) ;
#6379 = VECTOR ( 'NONE', #10460, 1000.000000000000227 ) ;
#6380 = CARTESIAN_POINT ( 'NONE',  ( 0.5972649247965632346, 12.28758346551315661, 4.089179521135787532 ) ) ;
#6381 = EDGE_CURVE ( 'NONE', #15355, #21755, #4242, .T. ) ;
#6382 = CARTESIAN_POINT ( 'NONE',  ( -47.86112874365709047, -10.87373999999999974, -23.29368419115692035 ) ) ;
#6383 = ORIENTED_EDGE ( 'NONE', *, *, #964, .T. ) ;
#6384 = ADVANCED_FACE ( 'NONE', ( #5021 ), #11776, .T. ) ;
#6385 = VECTOR ( 'NONE', #932, 1000.000000000000000 ) ;
#6386 = CARTESIAN_POINT ( 'NONE',  ( 4.000040237993640169, 12.73801256019466699, 1.129472658065480806 ) ) ;
#6387 = DIRECTION ( 'NONE',  ( 0.000000000000000000, 1.000000000000000000, 0.000000000000000000 ) ) ;
#6388 = PLANE ( 'NONE',  #1900 ) ;
#6389 = AXIS2_PLACEMENT_3D ( 'NONE', #8230, #13435, #150 ) ;
#6390 = CARTESIAN_POINT ( 'NONE',  ( 66.03921914090641110, 0.000000000000000000, -10.93409647675949969 ) ) ;
#6391 = CARTESIAN_POINT ( 'NONE',  ( 1.818456832593254191, 17.60937233235423349, -0.5547632684056083008 ) ) ;
#6392 = VECTOR ( 'NONE', #14910, 1000.000000000000000 ) ;
#6393 = ORIENTED_EDGE ( 'NONE', *, *, #18942, .T. ) ;
#6394 = VECTOR ( 'NONE', #5247, 1000.000000000000000 ) ;
#6395 = DIRECTION ( 'NONE',  ( -0.9685006480810792739, 0.000000000000000000, -0.2490110332224846346 ) ) ;
#6396 = DIRECTION ( 'NONE',  ( 0.000000000000000000, -1.000000000000000000, 0.000000000000000000 ) ) ;
#6397 = LINE ( 'NONE', #11487, #377 ) ;
#6398 = CARTESIAN_POINT ( 'NONE',  ( 53.10651001381376091, 37.69740999999999786, -16.70269254552787075 ) ) ;
#6399 = ORIENTED_EDGE ( 'NONE', *, *, #17925, .T. ) ;
#6400 = ORIENTED_EDGE ( 'NONE', *, *, #2874, .F. ) ;
#6401 = CARTESIAN_POINT ( 'NONE',  ( 8.907572712854108232, 13.29753225131360139, 6.491457205961016719 ) ) ;
#6402 = CARTESIAN_POINT ( 'NONE',  ( 40.38185354615648492, 38.88803500000000213, -3.606915520851464052 ) ) ;
#6403 = ORIENTED_EDGE ( 'NONE', *, *, #764, .F. ) ;
#6404 = EDGE_CURVE ( 'NONE', #14366, #7791, #20497, .T. ) ;
#6405 = VECTOR ( 'NONE', #15971, 1000.000000000000000 ) ;
#6406 = ORIENTED_EDGE ( 'NONE', *, *, #2312, .F. ) ;
#6407 = LINE ( 'NONE', #1539, #5309 ) ;
#6408 = CARTESIAN_POINT ( 'NONE',  ( 8.218225581203913777, 11.57903772877708093, 1.939056832797267704 ) ) ;
#6409 = AXIS2_PLACEMENT_3D ( 'NONE', #9413, #15854, #4117 ) ;
#6410 = AXIS2_PLACEMENT_3D ( 'NONE', #5438, #19265, #13990 ) ;
#6411 = EDGE_CURVE ( 'NONE', #9888, #21307, #13828, .T. ) ;
#6412 = AXIS2_PLACEMENT_3D ( 'NONE', #6743, #1441, #11616 ) ;
#6413 = EDGE_CURVE ( 'NONE', #1375, #5344, #8874, .T. ) ;
#6414 = CARTESIAN_POINT ( 'NONE',  ( -15.40791870427606369, 37.14670541160712958, -10.30897195908432451 ) ) ;
#6415 = CARTESIAN_POINT ( 'NONE',  ( 4.133078020274367326, 11.26694048801452119, 2.004190681395073170 ) ) ;
#6416 = CARTESIAN_POINT ( 'NONE',  ( 1.656824918492299847, 16.43570309294506870, 9.610848083271367415 ) ) ;
#6417 = DIRECTION ( 'NONE',  ( 0.8667647648559581031, 0.000000000000000000, 0.4987171968201974948 ) ) ;
#6418 = VERTEX_POINT ( 'NONE', #7240 ) ;
#6419 = CARTESIAN_POINT ( 'NONE',  ( 3.810589158948427535, 17.18860055147588994, -0.6831702454440164995 ) ) ;
#6420 = DIRECTION ( 'NONE',  ( -0.8609107660235850723, 0.000000000000000000, 0.5087559856598092844 ) ) ;
#6421 = CARTESIAN_POINT ( 'NONE',  ( 53.92979111630407374, -6.356984999999459873, -15.65141968182990162 ) ) ;
#6422 = CARTESIAN_POINT ( 'NONE',  ( 16.56531485685111349, -8.361256251594079814, -14.73559131467589545 ) ) ;
#6423 = DIRECTION ( 'NONE',  ( 1.000000000000000000, 0.000000000000000000, 0.000000000000000000 ) ) ;
#6424 = CIRCLE ( 'NONE', #15637, 0.7950200000000000600 ) ;
#6425 = ORIENTED_EDGE ( 'NONE', *, *, #967, .F. ) ;
#6426 = AXIS2_PLACEMENT_3D ( 'NONE', #20406, #15706, #7175 ) ;
#6427 = CARTESIAN_POINT ( 'NONE',  ( 10.33952242563266744, 21.01595720978967918, 5.389057817419801388 ) ) ;
#6428 = MANIFOLD_SOLID_BREP ( 'Stock-MAS-676-1', #9231 ) ;
#6429 = CARTESIAN_POINT ( 'NONE',  ( 9.951424491271426476, 20.70236077687740206, -1.727763842408016393 ) ) ;
#6430 = VERTEX_POINT ( 'NONE', #20469 ) ;
#6431 = EDGE_CURVE ( 'NONE', #9031, #14393, #3915, .T. ) ;
#6432 = EDGE_CURVE ( 'NONE', #8132, #21636, #17098, .T. ) ;
#6433 = ADVANCED_FACE ( 'NONE', ( #2361 ), #5336, .T. ) ;
#6434 = CARTESIAN_POINT ( 'NONE',  ( 6.842398409408770199, 21.43872775588835111, 1.301663748024633804 ) ) ;
#6435 = AXIS2_PLACEMENT_3D ( 'NONE', #15941, #14176, #12507 ) ;
#6436 = DIRECTION ( 'NONE',  ( -0.000000000000000000, -1.000000000000000000, 0.000000000000000000 ) ) ;
#6437 = CARTESIAN_POINT ( 'NONE',  ( 2.360830742822978667, 19.25518317520560174, 1.052360069546889987 ) ) ;
#6438 = CARTESIAN_POINT ( 'NONE',  ( 6.396056618077795797, 11.71523274630726164, 2.847703469759983008 ) ) ;
#6439 = CARTESIAN_POINT ( 'NONE',  ( 6.615032896206390234, 19.57687688253193770, 6.294354736441118980 ) ) ;
#6440 = DIRECTION ( 'NONE',  ( 0.000000000000000000, 1.000000000000000000, 0.000000000000000000 ) ) ;
#6441 = VECTOR ( 'NONE', #15137, 1000.000000000000000 ) ;
#6442 = CARTESIAN_POINT ( 'NONE',  ( 7.696359196369368050, 14.62096091062142023, -2.088485338917269729 ) ) ;
#6443 = CARTESIAN_POINT ( 'NONE',  ( 5.119829882126274434, 17.94946437092776392, 7.743928121518011132 ) ) ;
#6444 = DIRECTION ( 'NONE',  ( 0.7421532822901579785, 0.000000000000000000, -0.6702301885068630005 ) ) ;
#6445 = CARTESIAN_POINT ( 'NONE',  ( 2.063750000000000195, 24.21318500000000284, 8.731249999999999289 ) ) ;
#6446 = CARTESIAN_POINT ( 'NONE',  ( 7.711067097055989805, 13.03499949018002191, 7.247388574493073499 ) ) ;
#6447 = LINE ( 'NONE', #13102, #19530 ) ;
#6448 = AXIS2_PLACEMENT_3D ( 'NONE', #16744, #1583, #8327 ) ;
#6449 = CIRCLE ( 'NONE', #2199, 0.5953125000000004663 ) ;
#6450 = CARTESIAN_POINT ( 'NONE',  ( 54.55586098912687731, -9.531985000000000596, -6.056925149195119040 ) ) ;
#6451 = CARTESIAN_POINT ( 'NONE',  ( 6.468185970740263357, 11.70956081790287051, 2.825690715312092038 ) ) ;
#6452 = CARTESIAN_POINT ( 'NONE',  ( 39.72822375471606193, 39.64629009929521430, -3.182007191425374693 ) ) ;
#6453 = CARTESIAN_POINT ( 'NONE',  ( 21.24976161462477364, -2.911874215672294319, -15.04173616848670036 ) ) ;
#6454 = DIRECTION ( 'NONE',  ( 0.000000000000000000, 1.000000000000000000, 0.000000000000000000 ) ) ;
#6455 = ORIENTED_EDGE ( 'NONE', *, *, #10218, .T. ) ;
#6456 = PLANE ( 'NONE',  #11376 ) ;
#6457 = CARTESIAN_POINT ( 'NONE',  ( 11.15047342604716363, 13.70924040045908221, 6.092156091579346011 ) ) ;
#6458 = CARTESIAN_POINT ( 'NONE',  ( 57.35354854712898742, 34.52875999999999834, -21.22263945788050776 ) ) ;
#6459 = AXIS2_PLACEMENT_3D ( 'NONE', #11079, #14199, #579 ) ;
#6460 = VERTEX_POINT ( 'NONE', #17515 ) ;
#6461 = EDGE_CURVE ( 'NONE', #2495, #9790, #9176, .T. ) ;
#6462 = CARTESIAN_POINT ( 'NONE',  ( 12.81596010970969068, 18.61745565307525041, 5.882957067036275411 ) ) ;
#6463 = DIRECTION ( 'NONE',  ( 0.000000000000000000, 0.000000000000000000, -1.000000000000000000 ) ) ;
#6464 = CARTESIAN_POINT ( 'NONE',  ( -23.01875000000000071, 30.56064500000000095, -3.968750000000000000 ) ) ;
#6465 = CARTESIAN_POINT ( 'NONE',  ( 20.30874841272881781, -3.328473208352423995, -15.12328466456706266 ) ) ;
#6467 = CYLINDRICAL_SURFACE ( 'NONE', #8814, 30.16250000000000142 ) ;
#6466 = CARTESIAN_POINT ( 'NONE',  ( -0.9505311321298592908, 20.13283946025274318, 4.032600115501251636 ) ) ;
#6468 = EDGE_LOOP ( 'NONE', ( #3934, #4478, #7180, #1088 ) ) ;
#6469 = DIRECTION ( 'NONE',  ( 0.000000000000000000, 0.000000000000000000, 1.000000000000000000 ) ) ;
#6470 = CARTESIAN_POINT ( 'NONE',  ( -29.36874999999999858, 1.984375000000000000, 8.731249999999999289 ) ) ;
#6471 = ORIENTED_EDGE ( 'NONE', *, *, #4405, .T. ) ;
#6472 = VECTOR ( 'NONE', #20341, 1000.000000000000114 ) ;
#6473 = CARTESIAN_POINT ( 'NONE',  ( 53.10651001381376091, -7.547610000000002373, -16.70269254552787075 ) ) ;
#6474 = CARTESIAN_POINT ( 'NONE',  ( 0.4093006246296175821, 18.44896716303925643, 1.333896071427123076 ) ) ;
#6475 = CARTESIAN_POINT ( 'NONE',  ( 21.04230988742212460, -1.217322810690986357, -15.63980871831360098 ) ) ;
#6476 = VERTEX_POINT ( 'NONE', #14104 ) ;
#6477 = CARTESIAN_POINT ( 'NONE',  ( 9.237080217971490370, 15.41846441754162456, -2.863985544511726378 ) ) ;
#6478 = CARTESIAN_POINT ( 'NONE',  ( 3.009791520067166104, 20.22182912478766426, 2.433118109139212226 ) ) ;
#6479 = CARTESIAN_POINT ( 'NONE',  ( 42.94469661997857912, 0.000000000000000000, -18.48251861828712705 ) ) ;
#6480 = CARTESIAN_POINT ( 'NONE',  ( 12.91314300807607474, 11.26870765665696084, 4.644675481207224621 ) ) ;
#6481 = CARTESIAN_POINT ( 'NONE',  ( 12.73876125567402084, -5.603651328527227804, -16.73694851094560221 ) ) ;
#6482 = CARTESIAN_POINT ( 'NONE',  ( 13.62051399351888747, 17.23237496650334677, -17.80340391586448234 ) ) ;
#6483 = AXIS2_PLACEMENT_3D ( 'NONE', #236, #13744, #5312 ) ;
#6484 = VERTEX_POINT ( 'NONE', #20586 ) ;
#6485 = CARTESIAN_POINT ( 'NONE',  ( 9.120425135976756081, 21.04856296946614336, 1.778270776082491622 ) ) ;
#6486 = CARTESIAN_POINT ( 'NONE',  ( 5.359841762299309309, 15.44500604033330404, -2.196771070663687375 ) ) ;
#6487 = DIRECTION ( 'NONE',  ( 0.1831666983862991482, 0.000000000000000000, -0.9830818687180954418 ) ) ;
#6488 = ORIENTED_EDGE ( 'NONE', *, *, #11943, .F. ) ;
#6489 = ORIENTED_EDGE ( 'NONE', *, *, #37, .T. ) ;
#6490 = ADVANCED_FACE ( 'NONE', ( #15869 ), #20807, .T. ) ;
#6491 = LINE ( 'NONE', #18214, #4962 ) ;
#6493 = DIRECTION ( 'NONE',  ( 0.3542738219355897056, 0.000000000000000000, 0.9351417320872542627 ) ) ;
#6492 = CARTESIAN_POINT ( 'NONE',  ( 3.312557453758251391, 18.28455830479323652, 8.964874161621944282 ) ) ;
#6494 = ORIENTED_EDGE ( 'NONE', *, *, #14416, .F. ) ;
#6495 = CARTESIAN_POINT ( 'NONE',  ( 6.345927281321680269, 20.98284991768050389, 5.697012443342495125 ) ) ;
#6496 = CIRCLE ( 'NONE', #16042, 0.5080000000000012284 ) ;
#6497 = ORIENTED_EDGE ( 'NONE', *, *, #14126, .F. ) ;
#6498 = ORIENTED_EDGE ( 'NONE', *, *, #16291, .T. ) ;
#6499 = EDGE_CURVE ( 'NONE', #21254, #14428, #5556, .T. ) ;
#6500 =( BOUNDED_CURVE ( )  B_SPLINE_CURVE ( 3, ( #6663, #13425, #13540, #9989 ),
 .UNSPECIFIED., .F., .T. ) 
 B_SPLINE_CURVE_WITH_KNOTS ( ( 4, 4 ),
 ( 0.9998823759999307947, 1.570796326793153508 ),
 .UNSPECIFIED. ) 
 CURVE ( )  GEOMETRIC_REPRESENTATION_ITEM ( )  RATIONAL_B_SPLINE_CURVE ( ( 1.000000000000000000, 0.9730220469484401891, 0.9730220469484401891, 1.000000000000000000 ) ) 
 REPRESENTATION_ITEM ( '' )  );
#6501 = CYLINDRICAL_SURFACE ( 'NONE', #14982, 0.3962400000000008138 ) ;
#6502 = ORIENTED_EDGE ( 'NONE', *, *, #16836, .T. ) ;
#6503 = VECTOR ( 'NONE', #13046, 1000.000000000000000 ) ;
#6504 = CARTESIAN_POINT ( 'NONE',  ( 13.37230979461818237, 18.77374700936764285, 6.607210930384802339 ) ) ;
#6505 = CARTESIAN_POINT ( 'NONE',  ( 4.367181163445200909, 11.96053466636032248, 2.834654086721348776 ) ) ;
#6506 = CARTESIAN_POINT ( 'NONE',  ( 30.50878709810603340, 0.000000000000000000, -19.83971405306587954 ) ) ;
#6507 = AXIS2_PLACEMENT_3D ( 'NONE', #19172, #4252, #19051 ) ;
#6508 = FACE_OUTER_BOUND ( 'NONE', #21544, .T. ) ;
#6509 = PRODUCT ( 'Frame Locking Pawl Plate', 'Frame Locking Pawl Plate', '', ( #20468 ) ) ;
#6510 = FACE_OUTER_BOUND ( 'NONE', #6944, .T. ) ;
#6511 = CARTESIAN_POINT ( 'NONE',  ( 2.220423517640655042, 19.49008684387294110, 0.3265225556390483064 ) ) ;
#6512 = VERTEX_POINT ( 'NONE', #9092 ) ;
#6513 = CARTESIAN_POINT ( 'NONE',  ( 56.47666780297049627, 34.52875999999999834, 1.109116340531466127 ) ) ;
#6514 = CARTESIAN_POINT ( 'NONE',  ( 39.88301061098722755, 34.52875999999999834, -24.08706006053352411 ) ) ;
#6515 = CARTESIAN_POINT ( 'NONE',  ( -20.63749999999999929, 16.27314499999999953, 8.731249999999999289 ) ) ;
#6516 = FACE_OUTER_BOUND ( 'NONE', #15537, .T. ) ;
#6517 = ORIENTED_EDGE ( 'NONE', *, *, #17057, .F. ) ;
#6518 = ORIENTED_EDGE ( 'NONE', *, *, #20540, .F. ) ;
#6519 = EDGE_CURVE ( 'NONE', #18557, #3519, #697, .T. ) ;
#6520 = CARTESIAN_POINT ( 'NONE',  ( 6.640128354688219048, 20.89828364148222306, 1.681561550837193053 ) ) ;
#6521 = EDGE_CURVE ( 'NONE', #1632, #7768, #3923, .T. ) ;
#6522 = CARTESIAN_POINT ( 'NONE',  ( 6.016625000000000334, 32.54502000000000095, 2.794000000000000039 ) ) ;
#6523 = VECTOR ( 'NONE', #1890, 1000.000000000000114 ) ;
#6524 = ORIENTED_EDGE ( 'NONE', *, *, #13177, .F. ) ;
#6525 = ORIENTED_EDGE ( 'NONE', *, *, #9623, .T. ) ;
#6526 = DIRECTION ( 'NONE',  ( 0.000000000000000000, 1.000000000000000000, 0.000000000000000000 ) ) ;
#6527 = CARTESIAN_POINT ( 'NONE',  ( 8.778734981106474322, 11.92537842860997266, 4.412194450849771243 ) ) ;
#6528 = AXIS2_PLACEMENT_3D ( 'NONE', #15822, #21093, #4084 ) ;
#6529 = CARTESIAN_POINT ( 'NONE',  ( 7.062963379299048938, 12.66652504735844609, 5.873350661943272044 ) ) ;
#6530 = CARTESIAN_POINT ( 'NONE',  ( -53.00154558624916490, -10.87373999999999974, -22.85927301266823264 ) ) ;
#6531 = ADVANCED_FACE ( 'NONE', ( #4354 ), #11196, .F. ) ;
#6532 = DIRECTION ( 'NONE',  ( 0.9784543669157947932, 0.000000000000000000, 0.2064631973582977953 ) ) ;
#6533 = CARTESIAN_POINT ( 'NONE',  ( 7.106325486155565585, 11.65952799072720047, 6.014680116311857283 ) ) ;
#6534 = CARTESIAN_POINT ( 'NONE',  ( 0.1952384575209598350, 18.78947810346299718, 0.6406485339171671400 ) ) ;
#6535 = CYLINDRICAL_SURFACE ( 'NONE', #15130, 5.158739999999997217 ) ;
#6536 = ORIENTED_EDGE ( 'NONE', *, *, #21577, .T. ) ;
#6537 = CARTESIAN_POINT ( 'NONE',  ( 3.543013425253076054, 14.97059756667285058, 8.287472907696502133 ) ) ;
#6538 = DIRECTION ( 'NONE',  ( 0.000000000000000000, -1.000000000000000000, 0.000000000000000000 ) ) ;
#6539 = CARTESIAN_POINT ( 'NONE',  ( 67.40134256979101224, 30.56064500000000095, -13.70358117861468017 ) ) ;
#6540 = VECTOR ( 'NONE', #16786, 1000.000000000000114 ) ;
#6541 = ORIENTED_EDGE ( 'NONE', *, *, #17264, .F. ) ;
#6542 = ADVANCED_FACE ( 'NONE', ( #12765 ), #9316, .F. ) ;
#6543 = CARTESIAN_POINT ( 'NONE',  ( 12.84123145286963563, 11.26511959538250096, 4.668661225537280579 ) ) ;
#6544 = EDGE_CURVE ( 'NONE', #13842, #11503, #7664, .T. ) ;
#6545 = CARTESIAN_POINT ( 'NONE',  ( 9.172305780378046336, 17.26398718446571223, -3.555164033155447267 ) ) ;
#6546 = ORIENTED_EDGE ( 'NONE', *, *, #13409, .F. ) ;
#6547 = CARTESIAN_POINT ( 'NONE',  ( 9.025443331680945036, 19.27445160448637296, 7.159428889452720490 ) ) ;
#6548 = DIRECTION ( 'NONE',  ( 0.000000000000000000, 1.000000000000000000, 0.000000000000000000 ) ) ;
#6549 = CARTESIAN_POINT ( 'NONE',  ( 5.279567021499281587, 14.21946822237472752, 7.642569973796522476 ) ) ;
#6550 =( NAMED_UNIT ( * ) PLANE_ANGLE_UNIT ( ) SI_UNIT ( $, .RADIAN. ) );
#6551 = DIRECTION ( 'NONE',  ( -0.9636276526537417286, 0.000000000000000000, 0.2672484743474501934 ) ) ;
#6552 = CARTESIAN_POINT ( 'NONE',  ( 5.932080435518681583, 13.78737461787913077, -1.327312924921903114 ) ) ;
#6553 = EDGE_CURVE ( 'NONE', #12688, #19126, #3227, .T. ) ;
#6554 = DIRECTION ( 'NONE',  ( 0.08420877549337300871, 0.000000000000000000, 0.9964481331860212121 ) ) ;
#6555 = CARTESIAN_POINT ( 'NONE',  ( 0.3694878298779649128, 20.96126479766088124, 6.369946474118858504 ) ) ;
#6556 = CARTESIAN_POINT ( 'NONE',  ( 66.03921914090641110, 0.000000000000000000, -10.93409647675949969 ) ) ;
#6557 = EDGE_CURVE ( 'NONE', #8141, #11451, #16089, .T. ) ;
#6558 = CARTESIAN_POINT ( 'NONE',  ( 28.56548256563643662, 34.52875999999999834, -12.12873025803960658 ) ) ;
#6559 = CARTESIAN_POINT ( 'NONE',  ( 6.757070482422969704, 11.22565637327918253, 2.703836977927735585 ) ) ;
#6560 = DIRECTION ( 'NONE',  ( 0.000000000000000000, 1.000000000000000000, 0.000000000000000000 ) ) ;
#6561 = DIRECTION ( 'NONE',  ( 0.000000000000000000, -1.000000000000000000, 0.000000000000000000 ) ) ;
#6562 = PLANE ( 'NONE',  #7154 ) ;
#6563 = CARTESIAN_POINT ( 'NONE',  ( 55.27198911326564001, -1.983739999999999837, 2.462719476673013830 ) ) ;
#6564 = ORIENTED_EDGE ( 'NONE', *, *, #12132, .T. ) ;
#6565 = CARTESIAN_POINT ( 'NONE',  ( 8.781357490942916399, 40.07707250000000698, -18.85455479843708559 ) ) ;
#6566 = CYLINDRICAL_SURFACE ( 'NONE', #11180, 9.524999999999998579 ) ;
#6567 = DIRECTION ( 'NONE',  ( 0.000000000000000000, 1.000000000000000000, -0.000000000000000000 ) ) ;
#6568 = CARTESIAN_POINT ( 'NONE',  ( 13.15388200968041055, 15.89351787639128233, 6.392798759906445305 ) ) ;
#6569 = CARTESIAN_POINT ( 'NONE',  ( 35.15748561355322011, 32.54502000000000095, 0.3244898641346534163 ) ) ;
#6570 = CARTESIAN_POINT ( 'NONE',  ( 17.38294349214931245, -7.258570677684963002, -14.09221851007123227 ) ) ;
#6571 = CARTESIAN_POINT ( 'NONE',  ( -13.18827588824692754, 32.54247999999999763, -0.8886449702404607409 ) ) ;
#6572 = ORIENTED_EDGE ( 'NONE', *, *, #18123, .T. ) ;
#6573 =( LENGTH_UNIT ( ) NAMED_UNIT ( * ) SI_UNIT ( .MILLI., .METRE. ) );
#6574 = DIRECTION ( 'NONE',  ( 0.9579671649362034858, 0.000000000000000000, -0.2868778675745011220 ) ) ;
#6575 = MANIFOLD_SOLID_BREP ( 'Stock-MAS-676-1', #8877 ) ;
#6576 = ORIENTED_EDGE ( 'NONE', *, *, #15998, .F. ) ;
#6577 = CARTESIAN_POINT ( 'NONE',  ( 6.010033701850474586, 11.35695304730319144, 2.937139218883811242 ) ) ;
#6578 = CARTESIAN_POINT ( 'NONE',  ( 12.46160258925475794, -5.743475608960900480, -17.28410787521212555 ) ) ;
#6579 = ORIENTED_EDGE ( 'NONE', *, *, #14771, .F. ) ;
#6580 = CARTESIAN_POINT ( 'NONE',  ( 10.10053423927090677, 20.26417264612534197, -1.196608788579085259 ) ) ;
#6581 = B_SPLINE_CURVE_WITH_KNOTS ( 'NONE', 3,
 ( #18529, #8901, #20276, #20380 ),
 .UNSPECIFIED., .F., .F.,
 ( 4, 4 ),
 ( 0.000000000000000000, 1.000000000000000000 ),
 .UNSPECIFIED. ) ;
#6582 = ADVANCED_FACE ( 'NONE', ( #21359 ), #12650, .T. ) ;
#6583 = CARTESIAN_POINT ( 'NONE',  ( 66.87634738983680904, 30.56064500000000095, 3.497859541731999755 ) ) ;
#6584 = EDGE_CURVE ( 'NONE', #15435, #2625, #19598, .T. ) ;
#6585 = CARTESIAN_POINT ( 'NONE',  ( 5.756884206421248429, 19.23872087217396398, -1.498017244082868960 ) ) ;
#6586 = CARTESIAN_POINT ( 'NONE',  ( 12.44019961867567936, -5.159552288755423710, -16.78848910152690621 ) ) ;
#6587 = DIRECTION ( 'NONE',  ( 0.000000000000000000, 1.000000000000000000, 0.000000000000000000 ) ) ;
#6588 = ORIENTED_EDGE ( 'NONE', *, *, #544, .F. ) ;
#6589 = CARTESIAN_POINT ( 'NONE',  ( 10.72300197756324103, 19.12441493153400174, 5.966615969704548661 ) ) ;
#6590 = CARTESIAN_POINT ( 'NONE',  ( 13.39295492035073920, 16.76849418036265149, 7.268524437313808484 ) ) ;
#6591 = CARTESIAN_POINT ( 'NONE',  ( -22.90596259062238005, 39.45064500000000152, -9.869321627248080375 ) ) ;
#6592 = ORIENTED_EDGE ( 'NONE', *, *, #7074, .T. ) ;
#6593 = VERTEX_POINT ( 'NONE', #9532 ) ;
#6594 = DIRECTION ( 'NONE',  ( 0.000000000000000000, -1.000000000000000000, -0.000000000000000000 ) ) ;
#6596 = DIRECTION ( 'NONE',  ( 0.000000000000000000, 1.000000000000000000, 0.000000000000000000 ) ) ;
#6595 = CARTESIAN_POINT ( 'NONE',  ( 0.1886871975376354371, 20.96126479766088124, 6.424089978990833671 ) ) ;
#6597 = VERTEX_POINT ( 'NONE', #3021 ) ;
#6598 = CARTESIAN_POINT ( 'NONE',  ( 4.697672132164100844, 20.97227537427880151, 1.222830952479448952 ) ) ;
#6599 = ORIENTED_EDGE ( 'NONE', *, *, #3048, .T. ) ;
#6600 = EDGE_LOOP ( 'NONE', ( #12483, #15620, #18280, #14881 ) ) ;
#6601 = DIRECTION ( 'NONE',  ( 0.000000000000000000, 1.000000000000000000, 0.000000000000000000 ) ) ;
#6602 = ORIENTED_EDGE ( 'NONE', *, *, #16336, .F. ) ;
#6603 = EDGE_CURVE ( 'NONE', #7901, #3268, #12985, .T. ) ;
#6604 = CARTESIAN_POINT ( 'NONE',  ( 6.128459561466241823, 11.10665485570860156, 1.321687314850935824 ) ) ;
#6605 = CARTESIAN_POINT ( 'NONE',  ( 30.47347900023190803, 37.11476346399999926, -8.148724574017967015 ) ) ;
#6606 = CARTESIAN_POINT ( 'NONE',  ( 34.72145145287101542, 32.54502000000000095, 0.5851394578805096947 ) ) ;
#6607 = CARTESIAN_POINT ( 'NONE',  ( 2.467395655297200729, 20.16159473827618243, 0.9463460702680616121 ) ) ;
#6608 = EDGE_LOOP ( 'NONE', ( #10510, #10284, #4936, #17903 ) ) ;
#6609 = CARTESIAN_POINT ( 'NONE',  ( 66.87634738983680904, 0.000000000000000000, 3.497859541731999755 ) ) ;
#6610 = LINE ( 'NONE', #13593, #8886 ) ;
#6611 = DIRECTION ( 'NONE',  ( 0.000000000000000000, -1.000000000000000000, -0.000000000000000000 ) ) ;
#6612 = ORIENTED_EDGE ( 'NONE', *, *, #6004, .T. ) ;
#6613 = VERTEX_POINT ( 'NONE', #19694 ) ;
#6614 = CARTESIAN_POINT ( 'NONE',  ( 10.67670849270701439, 19.10987469415690043, 6.120482877392228183 ) ) ;
#6615 = CARTESIAN_POINT ( 'NONE',  ( 38.54095024924464497, 38.88803500000000213, -2.295677052105690841 ) ) ;
#6616 = VERTEX_POINT ( 'NONE', #4564 ) ;
#6617 = ORIENTED_EDGE ( 'NONE', *, *, #18579, .T. ) ;
#6618 = FACE_OUTER_BOUND ( 'NONE', #501, .T. ) ;
#6619 =( BOUNDED_CURVE ( )  B_SPLINE_CURVE ( 3, ( #12551, #20935, #594, #15659 ),
 .UNSPECIFIED., .F., .F. ) 
 B_SPLINE_CURVE_WITH_KNOTS ( ( 4, 4 ),
 ( 4.712388980401398086, 6.283185307179586232 ),
 .UNSPECIFIED. ) 
 CURVE ( )  GEOMETRIC_REPRESENTATION_ITEM ( )  RATIONAL_B_SPLINE_CURVE ( ( 1.000000000000000000, 0.8047378541283031206, 0.8047378541283031206, 1.000000000000000000 ) ) 
 REPRESENTATION_ITEM ( '' )  );
#6620 = ORIENTED_EDGE ( 'NONE', *, *, #203, .T. ) ;
#6621 = CARTESIAN_POINT ( 'NONE',  ( 9.082171594463483544, 12.91581074416477115, 5.837840052964735627 ) ) ;
#6622 = EDGE_CURVE ( 'NONE', #18576, #7181, #6709, .T. ) ;
#6623 = CIRCLE ( 'NONE', #2026, 0.5080000000000022276 ) ;
#6624 = DIRECTION ( 'NONE',  ( -0.1132953773954069598, 0.7241889112991808375, -0.6802312681817410667 ) ) ;
#6625 = DIRECTION ( 'NONE',  ( 0.000000000000000000, -1.000000000000000000, 0.000000000000000000 ) ) ;
#6626 = CARTESIAN_POINT ( 'NONE',  ( 0.4730996965358145179, 19.72362395832615078, 1.304202306971568026 ) ) ;
#6627 = VERTEX_POINT ( 'NONE', #18055 ) ;
#6628 =( REPRESENTATION_RELATIONSHIP ('NONE','NONE', #15554, #560 ) REPRESENTATION_RELATIONSHIP_WITH_TRANSFORMATION ( #9090 )SHAPE_REPRESENTATION_RELATIONSHIP( ) );
#6629 = CARTESIAN_POINT ( 'NONE',  ( 7.098541355495150640, 12.34712571434790007, 5.562580927991336743 ) ) ;
#6630 = DIRECTION ( 'NONE',  ( -0.000000000000000000, -1.000000000000000000, 0.000000000000000000 ) ) ;
#6631 = DIRECTION ( 'NONE',  ( 0.7421532822901579785, -0.000000000000000000, -0.6702301885068630005 ) ) ;
#6632 = LINE ( 'NONE', #13622, #18426 ) ;
#6633 = EDGE_LOOP ( 'NONE', ( #7330, #14847, #21362, #17102, #458, #19988, #9054, #11106, #5248, #18635, #11826, #14362, #14352, #14492, #16802, #9448, #9344, #15406, #13002, #17947, #20029 ) ) ;
#6634 = CARTESIAN_POINT ( 'NONE',  ( 12.77646214304486527, 18.77374700936764285, 6.785646590749020213 ) ) ;
#6635 = MANIFOLD_SOLID_BREP ( 'Stock-MAS-676-1', #9939 ) ;
#6636 = LINE ( 'NONE', #3340, #16328 ) ;
#6637 = CARTESIAN_POINT ( 'NONE',  ( 12.41829272412508089, 20.89413022119176944, 5.033827648320388093 ) ) ;
#6638 = ORIENTED_EDGE ( 'NONE', *, *, #17505, .T. ) ;
#6639 = VECTOR ( 'NONE', #3831, 1000.000000000000114 ) ;
#6640 = CARTESIAN_POINT ( 'NONE',  ( 6.099948198004060629, 20.15547429746715125, -0.6732643854471319633 ) ) ;
#6641 = DIRECTION ( 'NONE',  ( -1.000000000000000000, 0.000000000000000000, 0.000000000000000000 ) ) ;
#6642 = DIRECTION ( 'NONE',  ( -1.000000000000000000, 0.000000000000000000, 0.000000000000000000 ) ) ;
#6643 = EDGE_CURVE ( 'NONE', #18042, #3414, #8829, .T. ) ;
#6644 = CARTESIAN_POINT ( 'NONE',  ( 6.256308338986228179, 11.80107813750363732, 2.226400015944866695 ) ) ;
#6645 = PLANE ( 'NONE',  #18862 ) ;
#6646 = ADVANCED_FACE ( 'NONE', ( #21693 ), #4883, .T. ) ;
#6647 = CARTESIAN_POINT ( 'NONE',  ( 49.79678389823170903, 32.54502000000000095, -28.13445659451038594 ) ) ;
#6648 = EDGE_CURVE ( 'NONE', #5980, #19395, #1423, .T. ) ;
#6649 = CARTESIAN_POINT ( 'NONE',  ( 6.294043155411415569, 19.02104356353402181, -1.302222655867340428 ) ) ;
#6650 = EDGE_CURVE ( 'NONE', #12037, #4819, #16825, .T. ) ;
#6651 = CARTESIAN_POINT ( 'NONE',  ( 5.228545106021627475, 13.24170083984223290, 6.829111360130051267 ) ) ;
#6652 = CARTESIAN_POINT ( 'NONE',  ( -15.39353573898878658, -4.587157632697119958, -10.30107656633069979 ) ) ;
#6653 = CARTESIAN_POINT ( 'NONE',  ( -0.07815241983022847005, 13.90637430850843081, 0.5352566576402777443 ) ) ;
#6654 = CARTESIAN_POINT ( 'NONE',  ( 53.69636427252483202, 38.88803500000000213, -18.48840734645144224 ) ) ;
#6655 = AXIS2_PLACEMENT_3D ( 'NONE', #19397, #4271, #9343 ) ;
#6656 = CARTESIAN_POINT ( 'NONE',  ( 52.96420052373725440, -1.983739999999999837, 7.017842122255405712 ) ) ;
#6657 = CARTESIAN_POINT ( 'NONE',  ( 1.342949756012494333, 17.16067149510373469, 8.863113058879841688 ) ) ;
#6658 = CARTESIAN_POINT ( 'NONE',  ( 36.51250000000000284, 1.984375000000000000, -10.31875000000000142 ) ) ;
#6659 = CARTESIAN_POINT ( 'NONE',  ( 11.75816929971251135, -6.239310308105337377, -16.98506567453073401 ) ) ;
#6660 = ORIENTED_EDGE ( 'NONE', *, *, #17146, .F. ) ;
#6661 = DIRECTION ( 'NONE',  ( 0.000000000000000000, -1.000000000000000000, -0.000000000000000000 ) ) ;
#6662 = CARTESIAN_POINT ( 'NONE',  ( 10.79420638430738855, 11.98813216246191793, 4.338092415360138787 ) ) ;
#6663 = CARTESIAN_POINT ( 'NONE',  ( -15.41509608936259035, -4.609114529603660415, -10.31276839742836415 ) ) ;
#6664 = AXIS2_PLACEMENT_3D ( 'NONE', #17846, #14101, #2581 ) ;
#6665 = ORIENTED_EDGE ( 'NONE', *, *, #3642, .F. ) ;
#6666 = CARTESIAN_POINT ( 'NONE',  ( 12.76598846464055192, 11.97584668644513606, 4.063973834900838966 ) ) ;
#6667 = CARTESIAN_POINT ( 'NONE',  ( -51.69815163306579819, -5.714999999999999858, -7.436124251198355850 ) ) ;
#6668 = CARTESIAN_POINT ( 'NONE',  ( 6.214991440876061368, 11.01927814362272251, 2.094123509549327355 ) ) ;
#6669 = CARTESIAN_POINT ( 'NONE',  ( 19.47373669678540509, -0.8724954979520347376, -15.45837838233364003 ) ) ;
#6670 = FACE_OUTER_BOUND ( 'NONE', #12910, .T. ) ;
#6671 = ORIENTED_EDGE ( 'NONE', *, *, #6354, .F. ) ;
#6672 = DIRECTION ( 'NONE',  ( 1.000000000000000000, 0.000000000000000000, 0.000000000000000000 ) ) ;
#6673 = EDGE_CURVE ( 'NONE', #12549, #17651, #8204, .T. ) ;
#6674 = CARTESIAN_POINT ( 'NONE',  ( -7.782183222552548685, -1.594802499995993328, -34.19446947474821741 ) ) ;
#6675 = DIRECTION ( 'NONE',  ( 0.000000000000000000, 1.000000000000000000, 0.000000000000000000 ) ) ;
#6676 = CIRCLE ( 'NONE', #15522, 0.5080000000000014504 ) ;
#6677 = CARTESIAN_POINT ( 'NONE',  ( 6.105958985786053006, 11.57849375196054176, 2.924589247399322911 ) ) ;
#6678 = PRODUCT_DEFINITION_SHAPE ( 'NONE', 'NONE',  #21883 ) ;
#6679 = VECTOR ( 'NONE', #2491, 1000.000000000000114 ) ;
#6680 = CARTESIAN_POINT ( 'NONE',  ( 10.63672918265855394, -3.118840168672979640, -17.63289682993426766 ) ) ;
#6681 = EDGE_LOOP ( 'NONE', ( #4075, #2413, #15806, #5465 ) ) ;
#6682 = CARTESIAN_POINT ( 'NONE',  ( 10.67714358499520522, 11.64784025693482228, 3.885139017224132019 ) ) ;
#6683 = EDGE_CURVE ( 'NONE', #1698, #8377, #13797, .T. ) ;
#6684 = CARTESIAN_POINT ( 'NONE',  ( 3.459290721496041776, 20.55082906393983322, 3.602416572006893691 ) ) ;
#6685 = AXIS2_PLACEMENT_3D ( 'NONE', #12991, #2916, #21582 ) ;
#6686 = CARTESIAN_POINT ( 'NONE',  ( 9.922397446926728648, 11.51584134576680363, 0.4461043797960159152 ) ) ;
#6687 = CARTESIAN_POINT ( 'NONE',  ( 38.96848998618624904, 37.69740999999999786, -3.934807454472129429 ) ) ;
#6688 = CARTESIAN_POINT ( 'NONE',  ( 6.011841773132246658, 11.11134465255707937, 1.358372952244610854 ) ) ;
#6689 = CARTESIAN_POINT ( 'NONE',  ( 15.64213961604280279, -7.230076693056714632, -16.15356297515639383 ) ) ;
#6690 = CYLINDRICAL_SURFACE ( 'NONE', #11661, 0.5953125000000004663 ) ;
#6691 = ORIENTED_EDGE ( 'NONE', *, *, #7853, .F. ) ;
#6692 = CARTESIAN_POINT ( 'NONE',  ( 8.793583754241840467, 20.84408765773402195, 0.9049662790635636389 ) ) ;
#6693 = CARTESIAN_POINT ( 'NONE',  ( 7.243059079953789947, 16.38024503317697622, -3.009810408447084473 ) ) ;
#6694 = ORIENTED_EDGE ( 'NONE', *, *, #13364, .F. ) ;
#6695 = ORIENTED_EDGE ( 'NONE', *, *, #10352, .T. ) ;
#6696 = DIRECTION ( 'NONE',  ( 0.000000000000000000, -1.000000000000000000, -0.000000000000000000 ) ) ;
#6697 = CARTESIAN_POINT ( 'NONE',  ( 11.60020922121511155, 20.23341255231735758, -2.977328076712147276 ) ) ;
#6698 = CIRCLE ( 'NONE', #19750, 1.191259999999999319 ) ;
#6700 = CARTESIAN_POINT ( 'NONE',  ( 12.88040283537677588, -6.754812500000002551, -0.09070320285213756550 ) ) ;
#6699 = CARTESIAN_POINT ( 'NONE',  ( 3.509209820245474898, 17.35406872798134259, -1.425442992431726452 ) ) ;
#6701 = VERTEX_POINT ( 'NONE', #19916 ) ;
#6702 = CARTESIAN_POINT ( 'NONE',  ( 7.237772546668600704, 18.50866281033818694, 7.944204046336037273 ) ) ;
#6703 = ADVANCED_FACE ( 'NONE', ( #16925 ), #13633, .T. ) ;
#6704 = AXIS2_PLACEMENT_3D ( 'NONE', #17160, #3356, #18692 ) ;
#6705 = EDGE_CURVE ( 'NONE', #7786, #17651, #16266, .T. ) ;
#6706 = ADVANCED_FACE ( 'NONE', ( #3233 ), #16615, .T. ) ;
#6707 = ORIENTED_EDGE ( 'NONE', *, *, #2393, .T. ) ;
#6708 = CARTESIAN_POINT ( 'NONE',  ( 0.09188070044341151155, 13.96121064407340739, 1.549658560270714025 ) ) ;
#6709 = CIRCLE ( 'NONE', #4956, 0.7950200000000007261 ) ;
#6710 = DIRECTION ( 'NONE',  ( -0.9790635044817341814, 0.000000000000000000, 0.2035550397114869736 ) ) ;
#6711 = ORIENTED_EDGE ( 'NONE', *, *, #7383, .F. ) ;
#6712 = CARTESIAN_POINT ( 'NONE',  ( 1.967132827584114008, 13.73989441795974287, 0.9368391563488658313 ) ) ;
#6713 = AXIS2_PLACEMENT_3D ( 'NONE', #13644, #3361, #20240 ) ;
#6714 = CARTESIAN_POINT ( 'NONE',  ( -51.02421882195815783, 41.43438499999999891, -23.02637480153789795 ) ) ;
#6715 = CARTESIAN_POINT ( 'NONE',  ( 42.27821610176829381, 0.000000000000000000, 7.496956594510385763 ) ) ;
#6716 = AXIS2_PLACEMENT_3D ( 'NONE', #18518, #18617, #20372 ) ;
#6717 = DIRECTION ( 'NONE',  ( 0.08420877549337300871, 0.000000000000000000, 0.9964481331860212121 ) ) ;
#6718 = CARTESIAN_POINT ( 'NONE',  ( 1.800420485084554656, 13.16437343919289660, 0.4094432821608885997 ) ) ;
#6719 = VERTEX_POINT ( 'NONE', #14977 ) ;
#6720 = CARTESIAN_POINT ( 'NONE',  ( 9.828862065001116477, 36.51313500000000545, -16.12522240043857025 ) ) ;
#6721 = LINE ( 'NONE', #18548, #5617 ) ;
#6722 = ORIENTED_EDGE ( 'NONE', *, *, #6521, .T. ) ;
#6723 = ORIENTED_EDGE ( 'NONE', *, *, #2518, .T. ) ;
#6724 = CARTESIAN_POINT ( 'NONE',  ( 7.934317618220886104, 19.55588805595618140, -1.064466008449746592 ) ) ;
#6725 = VECTOR ( 'NONE', #11063, 1000.000000000000000 ) ;
#6726 = PLANE ( 'NONE',  #12969 ) ;
#6727 = ORIENTED_EDGE ( 'NONE', *, *, #16187, .F. ) ;
#6728 = VERTEX_POINT ( 'NONE', #8309 ) ;
#6729 = EDGE_CURVE ( 'NONE', #2932, #11624, #6874, .T. ) ;
#6730 = CARTESIAN_POINT ( 'NONE',  ( -12.30312499704650087, 1.984216250000054860, 10.71562498306123956 ) ) ;
#6731 = VERTEX_POINT ( 'NONE', #21578 ) ;
#6732 = CIRCLE ( 'NONE', #19079, 3.174999999999999378 ) ;
#6733 = AXIS2_PLACEMENT_3D ( 'NONE', #6986, #3793, #5118 ) ;
#6734 = CARTESIAN_POINT ( 'NONE',  ( 9.260356396371024701, 15.85449124615785976, 7.206070117100887629 ) ) ;
#6735 = AXIS2_PLACEMENT_3D ( 'NONE', #20577, #17506, #10648 ) ;
#6736 = CIRCLE ( 'NONE', #7441, 30.16249999999998721 ) ;
#6737 = LINE ( 'NONE', #5283, #20596 ) ;
#6738 = DIRECTION ( 'NONE',  ( 0.000000000000000000, 1.000000000000000000, 0.000000000000000000 ) ) ;
#6739 = CARTESIAN_POINT ( 'NONE',  ( 0.2450306102960222998, 18.98085523423504739, 0.7556970042913269126 ) ) ;
#6740 = CARTESIAN_POINT ( 'NONE',  ( 19.79515554403045741, 36.51313500000000545, -10.69562145279641996 ) ) ;
#6741 = ORIENTED_EDGE ( 'NONE', *, *, #8716, .F. ) ;
#6742 = CARTESIAN_POINT ( 'NONE',  ( 0.7434690279575192351, 12.30129727290108121, 3.312830165727216336 ) ) ;
#6743 = CARTESIAN_POINT ( 'NONE',  ( 65.67421548912699336, 0.000000000000000000, -10.93409647675949969 ) ) ;
#6744 = CARTESIAN_POINT ( 'NONE',  ( 9.256853431388732290, 34.52875999999999834, -17.09316853730597074 ) ) ;
#6745 = DIRECTION ( 'NONE',  ( 0.000000000000000000, 1.000000000000000000, 0.000000000000000000 ) ) ;
#6746 = VECTOR ( 'NONE', #7108, 1000.000000000000000 ) ;
#6747 = LINE ( 'NONE', #21567, #13739 ) ;
#6748 = EDGE_LOOP ( 'NONE', ( #18825, #14326, #21435, #8986 ) ) ;
#6749 = CARTESIAN_POINT ( 'NONE',  ( 10.85821570307754946, 12.08730048838598314, 5.903571453362351562 ) ) ;
#6750 = CARTESIAN_POINT ( 'NONE',  ( 12.00567213455676452, 21.57614686056444953, 3.916759121994844328 ) ) ;
#6751 = ORIENTED_EDGE ( 'NONE', *, *, #12132, .F. ) ;
#6752 = AXIS2_PLACEMENT_3D ( 'NONE', #2467, #7435, #7112 ) ;
#6753 = EDGE_CURVE ( 'NONE', #5934, #10166, #7783, .T. ) ;
#6754 = VECTOR ( 'NONE', #21840, 1000.000000000000114 ) ;
#6755 = CARTESIAN_POINT ( 'NONE',  ( 9.479939784920428991, 14.42918437847127144, 7.660713865854686055 ) ) ;
#6756 = CARTESIAN_POINT ( 'NONE',  ( 0.4361718258524748815, 18.57760016544011705, 1.300908314747322825 ) ) ;
#6757 = DIRECTION ( 'NONE',  ( 0.000000000000000000, 1.000000000000000000, 0.000000000000000000 ) ) ;
#6758 = DIRECTION ( 'NONE',  ( -0.8583349619704310207, 0.000000000000000000, 0.5130897514657826175 ) ) ;
#6759 = CARTESIAN_POINT ( 'NONE',  ( 7.312436962488203740, 15.85013007038090649, 7.611556540862124187 ) ) ;
#6760 = CIRCLE ( 'NONE', #10652, 1.191259999999999097 ) ;
#6761 = CARTESIAN_POINT ( 'NONE',  ( 1.670997140563193373, -1.594802499999999013, -22.76294857149378714 ) ) ;
#6762 = ADVANCED_FACE ( 'NONE', ( #18687 ), #13205, .F. ) ;
#6763 = CARTESIAN_POINT ( 'NONE',  ( 6.499174407287954480, 11.49185006667808118, 1.355446987389384850 ) ) ;
#6764 = CARTESIAN_POINT ( 'NONE',  ( 3.643499464412459421, 13.65298187125114282, -0.8458288619479169546 ) ) ;
#6765 = DIRECTION ( 'NONE',  ( 0.000000000000000000, 1.000000000000000000, 0.000000000000000000 ) ) ;
#6766 = CARTESIAN_POINT ( 'NONE',  ( 19.76004621270132589, 0.003678105342030234953, -14.87712536579863887 ) ) ;
#6767 = CARTESIAN_POINT ( 'NONE',  ( 4.933961842320149671, 18.75973248553390604, 7.440319485191550619 ) ) ;
#6768 = LINE ( 'NONE', #11864, #10803 ) ;
#6769 = CARTESIAN_POINT ( 'NONE',  ( 11.05988272033677333, -4.938043300071689679, -17.11035408892384524 ) ) ;
#6770 = CYLINDRICAL_SURFACE ( 'NONE', #2854, 0.7950199999999982836 ) ;
#6771 = AXIS2_PLACEMENT_3D ( 'NONE', #14822, #4311, #17806 ) ;
#6772 = EDGE_LOOP ( 'NONE', ( #6820, #689, #17986, #3496 ) ) ;
#6773 = VECTOR ( 'NONE', #656, 1000.000000000000000 ) ;
#6774 = CARTESIAN_POINT ( 'NONE',  ( 11.05115549428196253, 12.98897226662114157, 5.556954956783895838 ) ) ;
#6775 = CARTESIAN_POINT ( 'NONE',  ( 11.05569795298371716, 18.99266784705168831, 6.938303826124779583 ) ) ;
#6776 = CYLINDRICAL_SURFACE ( 'NONE', #1640, 1.190624999999997824 ) ;
#6777 = VERTEX_POINT ( 'NONE', #14861 ) ;
#6778 = EDGE_CURVE ( 'NONE', #14025, #1010, #12092, .T. ) ;
#6779 = CARTESIAN_POINT ( 'NONE',  ( 12.48283250700034763, 11.39445025475912132, 2.811724565135549359 ) ) ;
#6780 = DIRECTION ( 'NONE',  ( 0.000000000000000000, 0.000000000000000000, -1.000000000000000000 ) ) ;
#6781 = EDGE_CURVE ( 'NONE', #4180, #15382, #17037, .T. ) ;
#6782 = CARTESIAN_POINT ( 'NONE',  ( 14.35383053111052476, 1.091503432583336153, -15.81152456092466174 ) ) ;
#6784 = CARTESIAN_POINT ( 'NONE',  ( 27.87822510359947614, 34.52875999999999834, -8.893823290944665061 ) ) ;
#6783 = CARTESIAN_POINT ( 'NONE',  ( 2.855769952450744054, 12.51757774536594070, 6.616514325381632311 ) ) ;
#6785 = ORIENTED_EDGE ( 'NONE', *, *, #16533, .T. ) ;
#6786 = DIRECTION ( 'NONE',  ( 0.000000000000000000, 0.000000000000000000, 1.000000000000000000 ) ) ;
#6787 = DIRECTION ( 'NONE',  ( -0.2868778675745011220, 0.000000000000000000, -0.9579671649362033747 ) ) ;
#6788 = VECTOR ( 'NONE', #9129, 1000.000000000000114 ) ;
#6789 = DIRECTION ( 'NONE',  ( 0.000000000000000000, 1.000000000000000000, 0.000000000000000000 ) ) ;
#6790 = VECTOR ( 'NONE', #20769, 1000.000000000000114 ) ;
#6791 = DIRECTION ( 'NONE',  ( 0.000000000000000000, -1.000000000000000000, 0.000000000000000000 ) ) ;
#6792 = ORIENTED_EDGE ( 'NONE', *, *, #16578, .F. ) ;
#6793 = CIRCLE ( 'NONE', #11744, 3.174999999999998934 ) ;
#6794 = CARTESIAN_POINT ( 'NONE',  ( 12.40836789703437759, 11.21920808676120274, 2.564551607113802589 ) ) ;
#6795 = CARTESIAN_POINT ( 'NONE',  ( 3.051097452952215683, 20.26740773906408322, 2.539636754529451146 ) ) ;
#6796 = CARTESIAN_POINT ( 'NONE',  ( 12.82150885573869026, 11.94669871286416196, 4.209032338432463938 ) ) ;
#6797 = CARTESIAN_POINT ( 'NONE',  ( 5.701977129479173456, 12.65090407144326257, 6.796530866308510888 ) ) ;
#6798 = CARTESIAN_POINT ( 'NONE',  ( 10.40241334969972264, 21.01184353768176294, 5.367285860140727394 ) ) ;
#6799 = EDGE_CURVE ( 'NONE', #19334, #14145, #15011, .T. ) ;
#6800 = AXIS2_PLACEMENT_3D ( 'NONE', #2003, #7100, #13531 ) ;
#6801 = CARTESIAN_POINT ( 'NONE',  ( 12.11282701178822307, -1.606571398329030620, -16.69983038620819826 ) ) ;
#6802 = CARTESIAN_POINT ( 'NONE',  ( 9.256853431388732290, -3.968114999999999615, -17.09316853730597074 ) ) ;
#6803 = ORIENTED_EDGE ( 'NONE', *, *, #15440, .T. ) ;
#6804 = CARTESIAN_POINT ( 'NONE',  ( 10.92372992060199799, 18.30785699476917827, 6.420144728694466174 ) ) ;
#6805 = CARTESIAN_POINT ( 'NONE',  ( 9.160249483111522650, 13.32481467742428016, -2.920332793413628281 ) ) ;
#6806 = ORIENTED_EDGE ( 'NONE', *, *, #9240, .T. ) ;
#6807 = ORIENTED_EDGE ( 'NONE', *, *, #17760, .F. ) ;
#6808 = FACE_OUTER_BOUND ( 'NONE', #3527, .T. ) ;
#6809 = CARTESIAN_POINT ( 'NONE',  ( 11.20169135129352789, 18.59438219489337740, -3.945768465746844367 ) ) ;
#6810 = VECTOR ( 'NONE', #19023, 1000.000000000000000 ) ;
#6811 = EDGE_CURVE ( 'NONE', #17559, #2599, #10612, .T. ) ;
#6813 = CARTESIAN_POINT ( 'NONE',  ( 20.38332674228396613, -1.359449706705494920, -15.33066107936057065 ) ) ;
#6812 = CARTESIAN_POINT ( 'NONE',  ( -0.6214517246260686800, 21.02721105424156178, 4.868466575270438135 ) ) ;
#6814 = VERTEX_POINT ( 'NONE', #10625 ) ;
#6815 = CARTESIAN_POINT ( 'NONE',  ( 6.898105259049923887, 19.81015148077474919, 7.136496755853531049 ) ) ;
#6816 = CYLINDRICAL_SURFACE ( 'NONE', #21827, 1.983739999999999393 ) ;
#6817 = ORIENTED_EDGE ( 'NONE', *, *, #18997, .T. ) ;
#6818 = CARTESIAN_POINT ( 'NONE',  ( 0.4630128912319489976, 12.46612062059815251, 3.460377433718159423 ) ) ;
#6819 = DIRECTION ( 'NONE',  ( 0.000000000000000000, -1.000000000000000000, 0.000000000000000000 ) ) ;
#6820 = ORIENTED_EDGE ( 'NONE', *, *, #261, .T. ) ;
#6821 = CARTESIAN_POINT ( 'NONE',  ( 2.015936624292824053, 13.40476583923045162, 1.212685581759113340 ) ) ;
#6822 = CIRCLE ( 'NONE', #10718, 0.7950199999999993938 ) ;
#6823 = LINE ( 'NONE', #10362, #20531 ) ;
#6824 = CARTESIAN_POINT ( 'NONE',  ( 30.42699695299585017, -3.968114999999999615, -4.832012189960551041 ) ) ;
#6825 = EDGE_CURVE ( 'NONE', #14729, #18381, #7084, .T. ) ;
#6826 = CARTESIAN_POINT ( 'NONE',  ( 64.19677489640052670, 0.000000000000000000, -11.74367670905533423 ) ) ;
#6827 = CARTESIAN_POINT ( 'NONE',  ( 1.737391270568420465, 16.91513162182804209, -0.6717990871026022770 ) ) ;
#6828 = EDGE_CURVE ( 'NONE', #11451, #13089, #4256, .T. ) ;
#6829 = CARTESIAN_POINT ( 'NONE',  ( 26.59062499999999929, 5.953125000000000000, 8.731249999999999289 ) ) ;
#6830 = EDGE_CURVE ( 'NONE', #10784, #6991, #13971, .T. ) ;
#6831 = ORIENTED_EDGE ( 'NONE', *, *, #13897, .F. ) ;
#6832 = DIRECTION ( 'NONE',  ( 0.000000000000000000, 1.000000000000000000, 0.000000000000000000 ) ) ;
#6833 = PLANE ( 'NONE',  #7151 ) ;
#6834 = FACE_BOUND ( 'NONE', #21681, .T. ) ;
#6835 = CARTESIAN_POINT ( 'NONE',  ( 13.03688366823242539, 19.74207161212150297, -19.41788288235926885 ) ) ;
#6837 = CARTESIAN_POINT ( 'NONE',  ( 19.23620902706707625, -5.156408013795760858, -14.22105839913137437 ) ) ;
#6836 = DIRECTION ( 'NONE',  ( 0.9964481331860212121, 0.000000000000000000, -0.08420877549337300871 ) ) ;
#6838 = AXIS2_PLACEMENT_3D ( 'NONE', #14659, #2920, #13210 ) ;
#6839 = ORIENTED_EDGE ( 'NONE', *, *, #114, .F. ) ;
#6840 = VERTEX_POINT ( 'NONE', #13737 ) ;
#6841 = CARTESIAN_POINT ( 'NONE',  ( 10.02870747286891273, 20.26079639706886226, -1.172339910205614011 ) ) ;
#6843 = FACE_OUTER_BOUND ( 'NONE', #11614, .T. ) ;
#6842 = CARTESIAN_POINT ( 'NONE',  ( 5.667562314204174889, 21.64188095357850372, 3.777664677578456143 ) ) ;
#6844 = ORIENTED_EDGE ( 'NONE', *, *, #9397, .F. ) ;
#6845 = ORIENTED_EDGE ( 'NONE', *, *, #6158, .T. ) ;
#6846 = CARTESIAN_POINT ( 'NONE',  ( 49.09065990372640442, 0.000000000000000000, -26.70549589918839928 ) ) ;
#6847 = ORIENTED_EDGE ( 'NONE', *, *, #2240, .F. ) ;
#6848 = CARTESIAN_POINT ( 'NONE',  ( 9.239775580759724605, 14.16665682807454196, 6.724960839789129174 ) ) ;
#6849 = DIRECTION ( 'NONE',  ( 0.000000000000000000, 1.000000000000000000, 0.000000000000000000 ) ) ;
#6850 = CIRCLE ( 'NONE', #10373, 9.525000000000002132 ) ;
#6851 = CARTESIAN_POINT ( 'NONE',  ( 29.37324403177899868, 1.984375000000000000, -10.70578951775076071 ) ) ;
#6852 = ADVANCED_FACE ( 'NONE', ( #20668 ), #9063, .T. ) ;
#6853 = DIRECTION ( 'NONE',  ( 0.000000000000000000, 1.000000000000000000, 0.000000000000000000 ) ) ;
#6854 = CARTESIAN_POINT ( 'NONE',  ( -0.06155728683911870780, 13.26885766964012170, 1.106704240812302897 ) ) ;
#6855 = EDGE_CURVE ( 'NONE', #16499, #14487, #20463, .T. ) ;
#6856 = LINE ( 'NONE', #6740, #9455 ) ;
#6857 = ORIENTED_EDGE ( 'NONE', *, *, #843, .T. ) ;
#6858 = CARTESIAN_POINT ( 'NONE',  ( 6.170767000723442308, 12.01572996145620209, 1.412382460721507194 ) ) ;
#6859 = VECTOR ( 'NONE', #3269, 1000.000000000000114 ) ;
#6860 = LINE ( 'NONE', #6960, #14211 ) ;
#6861 = DIRECTION ( 'NONE',  ( 0.000000000000000000, 1.000000000000000000, 0.000000000000000000 ) ) ;
#6862 = CARTESIAN_POINT ( 'NONE',  ( 12.25799425556778388, -3.968114999999999615, 0.2069032437451798767 ) ) ;
#6863 = DIRECTION ( 'NONE',  ( -0.2490110332224846346, 0.000000000000000000, 0.9685006480810792739 ) ) ;
#6864 = EDGE_LOOP ( 'NONE', ( #4856, #11736, #16245, #6691, #16579, #1399 ) ) ;
#6865 = CARTESIAN_POINT ( 'NONE',  ( 13.47935068733434250, 22.20657701893900082, 2.459632543707202412 ) ) ;
#6866 = DIRECTION ( 'NONE',  ( -0.9964481331860209901, 0.000000000000000000, 0.08420877549337456303 ) ) ;
#6867 = CARTESIAN_POINT ( 'NONE',  ( 12.10789021220345241, 21.43823440121504120, 4.195907106397960717 ) ) ;
#6868 = EDGE_LOOP ( 'NONE', ( #13462, #5747, #12101, #10674 ) ) ;
#6869 = CIRCLE ( 'NONE', #3010, 15.47812499999999680 ) ;
#6870 = ORIENTED_EDGE ( 'NONE', *, *, #6643, .F. ) ;
#6871 = CARTESIAN_POINT ( 'NONE',  ( 9.406149962978091139, 13.41239259737459122, 7.189453753586981577 ) ) ;
#6872 = CARTESIAN_POINT ( 'NONE',  ( 4.031802018818064326, 20.53258833712626341, 5.054834409609300749 ) ) ;
#6873 = DIRECTION ( 'NONE',  ( -0.9037041334408600912, -0.3596272420165190775, -0.2323512126103423614 ) ) ;
#6874 = LINE ( 'NONE', #13311, #17674 ) ;
#6875 = CARTESIAN_POINT ( 'NONE',  ( 7.325542279612724528, 15.26830868317408019, 7.512093565127778483 ) ) ;
#6876 = LINE ( 'NONE', #13525, #161 ) ;
#6877 = CIRCLE ( 'NONE', #13549, 1.984375000000000000 ) ;
#6878 = CARTESIAN_POINT ( 'NONE',  ( 6.156360451388549926, 12.39088710148332062, -0.1838423150655557059 ) ) ;
#6879 = CIRCLE ( 'NONE', #19239, 22.02656249999999005 ) ;
#6880 = CARTESIAN_POINT ( 'NONE',  ( 5.668910838604148239, 13.84264232191805100, 8.284811746615043049 ) ) ;
#6881 = DIRECTION ( 'NONE',  ( 0.08420877549337300871, 0.000000000000000000, 0.9964481331860212121 ) ) ;
#6882 = ADVANCED_FACE ( 'NONE', ( #3887 ), #565, .T. ) ;
#6883 = CARTESIAN_POINT ( 'NONE',  ( 20.01429352998429323, -0.5059105927738452024, -14.81829418944272980 ) ) ;
#6884 = DIRECTION ( 'NONE',  ( 0.000000000000000000, 1.000000000000000000, 0.000000000000000000 ) ) ;
#6885 = DIRECTION ( 'NONE',  ( 0.000000000000000000, -1.000000000000000000, 0.000000000000000000 ) ) ;
#6886 = CARTESIAN_POINT ( 'NONE',  ( 16.40614462543630836, -8.411149092273442207, -15.98937562035452409 ) ) ;
#6887 = CARTESIAN_POINT ( 'NONE',  ( 11.32797118285666116, 17.32754504092519454, 7.499948195778106452 ) ) ;
#6888 = CARTESIAN_POINT ( 'NONE',  ( 22.22454659879084460, -1.983739999999999393, -13.75904720189594244 ) ) ;
#6889 = ORIENTED_EDGE ( 'NONE', *, *, #17854, .T. ) ;
#6890 = CARTESIAN_POINT ( 'NONE',  ( 13.11430928665658513, 13.86836039950025601, 5.796722067417751312 ) ) ;
#6891 = CARTESIAN_POINT ( 'NONE',  ( 11.62603409302100133, -3.109374932586516316, -16.94889309930612598 ) ) ;
#6892 = CARTESIAN_POINT ( 'NONE',  ( 3.155748942043203442, 20.73071249212684108, 3.672874311289710203 ) ) ;
#6893 = EDGE_LOOP ( 'NONE', ( #21095, #10979, #1809, #457 ) ) ;
#6894 = APPLICATION_PROTOCOL_DEFINITION ( 'draft international standard', 'automotive_design', 1998, #13863 ) ;
#6895 = LINE ( 'NONE', #20358, #739 ) ;
#6896 = DIRECTION ( 'NONE',  ( 0.2490110332224850231, 0.000000000000000000, -0.9685006480810791629 ) ) ;
#6897 = DIRECTION ( 'NONE',  ( 0.000000000000000000, 1.000000000000000000, 0.000000000000000000 ) ) ;
#6898 = ORIENTED_EDGE ( 'NONE', *, *, #15391, .F. ) ;
#6899 = CARTESIAN_POINT ( 'NONE',  ( 8.510511870354847019, 20.63131727706956298, 0.2009566961665696649 ) ) ;
#6900 = CARTESIAN_POINT ( 'NONE',  ( 3.560108861471142916, 20.57711495788742440, 3.866665624095278808 ) ) ;
#6901 = CARTESIAN_POINT ( 'NONE',  ( 10.78593073986782613, 19.11233889549468046, 6.091437666761631675 ) ) ;
#6902 = CARTESIAN_POINT ( 'NONE',  ( 5.440308256469632120, 21.03084409073214189, 1.977388168171128058 ) ) ;
#6903 = CARTESIAN_POINT ( 'NONE',  ( 9.756654189145164580, 21.83905339296156356, 3.605447077296963343 ) ) ;
#6904 = EDGE_CURVE ( 'NONE', #7279, #19333, #3777, .T. ) ;
#6905 = CARTESIAN_POINT ( 'NONE',  ( 36.54633153140314761, 34.52875999999999834, -9.516661413425623550 ) ) ;
#6906 = CIRCLE ( 'NONE', #14337, 0.7950200000000003930 ) ;
#6907 = ADVANCED_BREP_SHAPE_REPRESENTATION ( '', ( #13288, #2234 ), #5057 ) ;
#6908 = CARTESIAN_POINT ( 'NONE',  ( 11.88130483305368656, -3.258360441252182493, -16.83834492875844546 ) ) ;
#6909 = CARTESIAN_POINT ( 'NONE',  ( 52.44708915697334106, 0.000000000000000000, 4.020247972991190188 ) ) ;
#6910 = ORIENTED_EDGE ( 'NONE', *, *, #18562, .T. ) ;
#6911 = CARTESIAN_POINT ( 'NONE',  ( 8.231392512103436587, 19.97299568257830060, -0.5599668506537556212 ) ) ;
#6912 = CARTESIAN_POINT ( 'NONE',  ( 9.082225001358835925, 11.50047795576720233, 5.498903420274817933 ) ) ;
#6913 = ORIENTED_EDGE ( 'NONE', *, *, #19245, .F. ) ;
#6914 = DIRECTION ( 'NONE',  ( -0.9685006480810792739, 0.000000000000000000, -0.2490110332224850509 ) ) ;
#6915 = FACE_OUTER_BOUND ( 'NONE', #15673, .T. ) ;
#6917 = DIRECTION ( 'NONE',  ( 0.000000000000000000, 1.000000000000000000, 0.000000000000000000 ) ) ;
#6916 = CARTESIAN_POINT ( 'NONE',  ( 1.365433128829952825, 14.65425108942523558, -0.3328239235251538308 ) ) ;
#6918 = ORIENTED_EDGE ( 'NONE', *, *, #1288, .F. ) ;
#6919 = CARTESIAN_POINT ( 'NONE',  ( 7.490479816045854555, 16.63476421355041879, 8.383926577843272554 ) ) ;
#6920 = VERTEX_POINT ( 'NONE', #12182 ) ;
#6921 = EDGE_CURVE ( 'NONE', #7865, #6840, #15407, .T. ) ;
#6922 = CARTESIAN_POINT ( 'NONE',  ( 0.4729859817002137201, 12.44863435665195084, 3.507523896227905613 ) ) ;
#6923 = DIRECTION ( 'NONE',  ( 0.000000000000000000, 1.000000000000000000, 0.000000000000000000 ) ) ;
#6924 = VERTEX_POINT ( 'NONE', #229 ) ;
#6925 = EDGE_CURVE ( 'NONE', #10936, #5639, #14073, .T. ) ;
#6926 = EDGE_CURVE ( 'NONE', #374, #19312, #666, .T. ) ;
#6927 = EDGE_CURVE ( 'NONE', #1, #10166, #5642, .T. ) ;
#6928 = DIRECTION ( 'NONE',  ( 0.9129422336036140395, 0.000000000000000000, -0.4080888115384250225 ) ) ;
#6929 = DIRECTION ( 'NONE',  ( 0.000000000000000000, 1.000000000000000000, -0.000000000000000000 ) ) ;
#6930 = DIRECTION ( 'NONE',  ( 0.8583349619704303546, 0.000000000000000000, -0.5130897514657839498 ) ) ;
#6931 = CARTESIAN_POINT ( 'NONE',  ( 3.555789604696411477, 21.36866284792075987, 3.849869910478822987 ) ) ;
#6932 = CARTESIAN_POINT ( 'NONE',  ( 1.268730000000000135, 9.129395000000000593, 10.65596716962832069 ) ) ;
#6933 = ORIENTED_EDGE ( 'NONE', *, *, #12897, .F. ) ;
#6934 = CARTESIAN_POINT ( 'NONE',  ( 23.77193158452286781, 2.770822500000000854, -15.00033089984030887 ) ) ;
#6935 = DIRECTION ( 'NONE',  ( 0.000000000000000000, -1.000000000000000000, 0.000000000000000000 ) ) ;
#6936 = CARTESIAN_POINT ( 'NONE',  ( 17.29174454768425306, 2.431241120636982167, -15.13097126745110721 ) ) ;
#6938 = CARTESIAN_POINT ( 'NONE',  ( 19.51444747994706930, -4.586276125266755876, -14.17934498840143931 ) ) ;
#6937 = DIRECTION ( 'NONE',  ( 0.2490110332224848289, 0.000000000000000000, -0.9685006480810792739 ) ) ;
#6939 = VERTEX_POINT ( 'NONE', #20327 ) ;
#6940 = ORIENTED_EDGE ( 'NONE', *, *, #9616, .T. ) ;
#6941 = CARTESIAN_POINT ( 'NONE',  ( 6.315595396583606913, 20.04364414270774120, 0.2372624680991833601 ) ) ;
#6943 = CARTESIAN_POINT ( 'NONE',  ( 17.22522857595987844, 36.51313500000000545, -15.04442098945225403 ) ) ;
#6942 = CARTESIAN_POINT ( 'NONE',  ( 6.875778001922447480, 20.09399725779506340, 7.023170949626798887 ) ) ;
#6944 = EDGE_LOOP ( 'NONE', ( #148, #12725, #19644, #4954 ) ) ;
#6945 = ORIENTED_EDGE ( 'NONE', *, *, #336, .T. ) ;
#6946 = CARTESIAN_POINT ( 'NONE',  ( -51.69815163306579819, 38.26001999999999725, -7.436124251198355850 ) ) ;
#6947 = CIRCLE ( 'NONE', #21778, 0.5080000000000023386 ) ;
#6948 = ORIENTED_EDGE ( 'NONE', *, *, #14837, .F. ) ;
#6949 = ADVANCED_FACE ( 'NONE', ( #10410 ), #17152, .T. ) ;
#6950 = CARTESIAN_POINT ( 'NONE',  ( 7.670747655007784438, 17.97917197181799764, -1.865092139437078300 ) ) ;
#6951 = ORIENTED_EDGE ( 'NONE', *, *, #14688, .F. ) ;
#6952 = ADVANCED_FACE ( 'NONE', ( #4324 ), #12618, .T. ) ;
#6953 = CARTESIAN_POINT ( 'NONE',  ( 11.75439013559175017, 34.52875999999999834, 4.331204221326972359 ) ) ;
#6954 = CARTESIAN_POINT ( 'NONE',  ( 61.09555596642878328, 34.52875999999999834, -12.53419992421059348 ) ) ;
#6955 = FACE_OUTER_BOUND ( 'NONE', #8872, .T. ) ;
#6956 = CARTESIAN_POINT ( 'NONE',  ( -0.03530231612252059809, 13.09097027921703749, 1.245598840680120167 ) ) ;
#6957 = CIRCLE ( 'NONE', #3430, 0.3962399999999998146 ) ;
#6958 = ORIENTED_EDGE ( 'NONE', *, *, #14628, .F. ) ;
#6959 = CARTESIAN_POINT ( 'NONE',  ( 1.638778877848424687, 13.09009564387116065, 7.486132227913222081 ) ) ;
#6960 = CARTESIAN_POINT ( 'NONE',  ( 38.82016491058538321, -9.531985000000000596, -14.75770094105646812 ) ) ;
#6961 = DIRECTION ( 'NONE',  ( 0.9724402360367340181, 0.000000000000000000, -0.2331522835762512846 ) ) ;
#6962 = LINE ( 'NONE', #20004, #11377 ) ;
#6963 = EDGE_LOOP ( 'NONE', ( #11701, #12234, #13162, #19409, #3322, #19301 ) ) ;
#6964 = CARTESIAN_POINT ( 'NONE',  ( 8.794480080286872337, 21.87018156742340125, 1.773917468153012322 ) ) ;
#6965 = DIRECTION ( 'NONE',  ( 0.000000000000000000, 1.000000000000000000, 0.000000000000000000 ) ) ;
#6966 = CARTESIAN_POINT ( 'NONE',  ( 11.60172015861852834, 21.94098819457760285, 2.803563881665107616 ) ) ;
#6967 = ORIENTED_EDGE ( 'NONE', *, *, #19213, .F. ) ;
#6968 = VERTEX_POINT ( 'NONE', #2766 ) ;
#6969 = CARTESIAN_POINT ( 'NONE',  ( 3.805353748838121053, 36.51313500000000545, -22.18284873352824960 ) ) ;
#6970 = CARTESIAN_POINT ( 'NONE',  ( 8.234954911211584516, 10.76337410253292148, 2.037235491473907700 ) ) ;
#6971 = CARTESIAN_POINT ( 'NONE',  ( 3.962787389995165110, 12.81957249642222152, 0.8790192768804812040 ) ) ;
#6972 = LINE ( 'NONE', #3780, #8048 ) ;
#6973 = EDGE_CURVE ( 'NONE', #11160, #19865, #15927, .T. ) ;
#6974 = CARTESIAN_POINT ( 'NONE',  ( 5.588254505849169718, 15.45064704472125250, -1.305107587893242105 ) ) ;
#6975 = ADVANCED_FACE ( 'NONE', ( #16273 ), #2665, .T. ) ;
#6976 = EDGE_CURVE ( 'NONE', #4294, #5857, #19341, .T. ) ;
#6977 = LINE ( 'NONE', #20335, #12171 ) ;
#6978 = CARTESIAN_POINT ( 'NONE',  ( -22.75431282566211522, -8.248365470396340271, -25.41543459098148716 ) ) ;
#6979 = CARTESIAN_POINT ( 'NONE',  ( 8.585932752112777067, 20.96234599748222038, 4.772909305667436541 ) ) ;
#6980 = CARTESIAN_POINT ( 'NONE',  ( 5.731357535509370216, 21.64685404058683815, 3.758912427147279356 ) ) ;
#6981 = CARTESIAN_POINT ( 'NONE',  ( -2.234700160307072192, 26.98019749999999917, -24.80708529208898483 ) ) ;
#6982 = DIRECTION ( 'NONE',  ( 0.000000000000000000, 1.000000000000000000, 0.000000000000000000 ) ) ;
#6983 = CARTESIAN_POINT ( 'NONE',  ( 1.941381905217177017, 13.53119643653954363, 0.9980600641242322046 ) ) ;
#6984 = PLANE ( 'NONE',  #20659 ) ;
#6985 = CARTESIAN_POINT ( 'NONE',  ( 11.17732588453249676, -0.8204807644301946867, -16.92579435541830080 ) ) ;
#6986 = CARTESIAN_POINT ( 'NONE',  ( 39.07078961959606289, 32.54502000000000095, -27.14892015257980162 ) ) ;
#6987 = AXIS2_PLACEMENT_3D ( 'NONE', #4212, #5764, #15626 ) ;
#6988 = CARTESIAN_POINT ( 'NONE',  ( 59.52193197173441774, 0.000000000000000000, -3.260183413611184911 ) ) ;
#6989 = CARTESIAN_POINT ( 'NONE',  ( 10.36888746642220305, 20.99033332477807079, 5.185665849892854951 ) ) ;
#6990 = DIRECTION ( 'NONE',  ( 0.000000000000000000, 1.000000000000000000, 0.000000000000000000 ) ) ;
#6991 = VERTEX_POINT ( 'NONE', #4208 ) ;
#6992 = CARTESIAN_POINT ( 'NONE',  ( 11.18318634076747742, 16.39223678439043397, -3.590085582233933259 ) ) ;
#6993 = LINE ( 'NONE', #11874, #3138 ) ;
#6994 = CARTESIAN_POINT ( 'NONE',  ( 3.931218227739150528, 11.94740837896324237, 2.317032250256635173 ) ) ;
#6995 = AXIS2_PLACEMENT_3D ( 'NONE', #11775, #8429, #16851 ) ;
#6996 = ORIENTED_EDGE ( 'NONE', *, *, #20699, .F. ) ;
#6997 = APPLICATION_PROTOCOL_DEFINITION ( 'draft international standard', 'automotive_design', 1998, #17231 ) ;
#6998 = DIRECTION ( 'NONE',  ( 1.000000000000000000, 0.000000000000000000, 0.000000000000000000 ) ) ;
#6999 = CARTESIAN_POINT ( 'NONE',  ( 4.520744627033614016, 19.76795696472709452, 0.8556426533025034420 ) ) ;
#7000 = EDGE_CURVE ( 'NONE', #10564, #20253, #2442, .T. ) ;
#7001 = CARTESIAN_POINT ( 'NONE',  ( -16.07247711516169275, -5.309201820043501385, -10.44681224123558039 ) ) ;
#7002 = CARTESIAN_POINT ( 'NONE',  ( 6.045917078792466093, 11.48351223332058346, 2.935635005282488663 ) ) ;
#7003 = VECTOR ( 'NONE', #11618, 1000.000000000000000 ) ;
#7004 = ORIENTED_EDGE ( 'NONE', *, *, #20453, .T. ) ;
#7005 = CARTESIAN_POINT ( 'NONE',  ( 9.544384125417266773, 12.37431098505726013, -1.081075134452434749 ) ) ;
#7006 = CARTESIAN_POINT ( 'NONE',  ( 3.265424270076857205, 20.45664453107361069, 3.095604235058887266 ) ) ;
#7007 = CARTESIAN_POINT ( 'NONE',  ( 6.745733615097072366, 11.82482810032952081, 4.272283726952619709 ) ) ;
#7008 = CARTESIAN_POINT ( 'NONE',  ( 5.789917961221411780, 17.41457342482845405, 8.273797100034885332 ) ) ;
#7009 = CARTESIAN_POINT ( 'NONE',  ( 13.23690675162799479, 12.74100552075486270, 6.152686933467335528 ) ) ;
#7010 = PLANE ( 'NONE',  #16065 ) ;
#7011 = PRODUCT_DEFINITION_CONTEXT ( 'detailed design', #19056, 'design' ) ;
#7012 = CARTESIAN_POINT ( 'NONE',  ( 11.26403972753813498, -4.566074002652793062, -15.20827691245368563 ) ) ;
#7013 = VERTEX_POINT ( 'NONE', #9168 ) ;
#7014 = CARTESIAN_POINT ( 'NONE',  ( 11.21878411960198463, 15.42120748821763598, 6.735290914777061211 ) ) ;
#7015 = CARTESIAN_POINT ( 'NONE',  ( 9.052665478973109359, 15.28237876918361948, -3.641785826635130174 ) ) ;
#7016 = ORIENTED_EDGE ( 'NONE', *, *, #11524, .T. ) ;
#7017 = CARTESIAN_POINT ( 'NONE',  ( 9.367590232042878995, 13.71580197176839633, -2.112308633255299384 ) ) ;
#7018 = CIRCLE ( 'NONE', #13042, 0.3962399999999988154 ) ;
#7019 = CARTESIAN_POINT ( 'NONE',  ( -47.86049599909252805, -8.889364999999999739, -23.29373766372935961 ) ) ;
#7020 = DIRECTION ( 'NONE',  ( 0.9685006480810791629, -4.068963411654120556E-16, 0.2490110332224850231 ) ) ;
#7022 = DIRECTION ( 'NONE',  ( 0.9790635044817341814, 0.000000000000000000, -0.2035550397114870014 ) ) ;
#7021 = CARTESIAN_POINT ( 'NONE',  ( 4.354639731569010408, 20.46779201619338195, 6.887242084015990251 ) ) ;
#7023 = ORIENTED_EDGE ( 'NONE', *, *, #4693, .T. ) ;
#7024 = CARTESIAN_POINT ( 'NONE',  ( 7.297179034909929030, 12.43031178068008558, 6.778800246622879833 ) ) ;
#7025 = EDGE_CURVE ( 'NONE', #13038, #21568, #21109, .T. ) ;
#7026 = CARTESIAN_POINT ( 'NONE',  ( 61.60152099976809126, 2.586003464000000029, -12.48877542598203405 ) ) ;
#7027 = ORIENTED_EDGE ( 'NONE', *, *, #21796, .F. ) ;
#7028 = ORIENTED_EDGE ( 'NONE', *, *, #7631, .F. ) ;
#7029 = CARTESIAN_POINT ( 'NONE',  ( 2.101062743772215580, 12.98372264194903636, 1.656677011360439877 ) ) ;
#7030 = CARTESIAN_POINT ( 'NONE',  ( 3.736893377926853610, 14.96998944597854653, -0.4414175379438642910 ) ) ;
#7031 = DIRECTION ( 'NONE',  ( -0.2868778675745008999, 0.000000000000000000, -0.9579671649362034858 ) ) ;
#7032 = CARTESIAN_POINT ( 'NONE',  ( 36.73521423675246922, -1.983739999999999837, 2.413462327205186497 ) ) ;
#7033 = CARTESIAN_POINT ( 'NONE',  ( 53.84486179190094646, -1.983739999999999837, -6.412645463410259872 ) ) ;
#7034 = CARTESIAN_POINT ( 'NONE',  ( 20.76310168089343478, 34.52875999999999834, -11.26763008640078212 ) ) ;
#7035 = CARTESIAN_POINT ( 'NONE',  ( 3.998154558026791872, 21.25887251078221496, 5.050199523078231501 ) ) ;
#7036 = DIRECTION ( 'NONE',  ( 1.000000000000000000, 0.000000000000000000, 0.000000000000000000 ) ) ;
#7037 = EDGE_LOOP ( 'NONE', ( #14220, #695, #11513, #4850 ) ) ;
#7038 = VECTOR ( 'NONE', #11177, 1000.000000000000000 ) ;
#7039 = LINE ( 'NONE', #1955, #20579 ) ;
#7040 = DIRECTION ( 'NONE',  ( -0.9784543669157944601, 0.000000000000000000, -0.2064631973582987667 ) ) ;
#7041 = DIRECTION ( 'NONE',  ( 0.000000000000000000, -1.000000000000000000, 0.000000000000000000 ) ) ;
#7042 = EDGE_CURVE ( 'NONE', #539, #7495, #17819, .T. ) ;
#7043 = CARTESIAN_POINT ( 'NONE',  ( 18.07371581377308800, 34.52875999999999834, -11.95909761906105473 ) ) ;
#7044 = AXIS2_PLACEMENT_3D ( 'NONE', #435, #5508, #7186 ) ;
#7046 = CARTESIAN_POINT ( 'NONE',  ( 19.00900242689141351, -5.516070221694524989, -14.25943734768673643 ) ) ;
#7045 = DIRECTION ( 'NONE',  ( 0.000000000000000000, 0.000000000000000000, -1.000000000000000000 ) ) ;
#7047 = ORIENTED_EDGE ( 'NONE', *, *, #13582, .F. ) ;
#7048 = ORIENTED_EDGE ( 'NONE', *, *, #18053, .F. ) ;
#7049 = CARTESIAN_POINT ( 'NONE',  ( 6.855085254147958551, 20.81034843036036008, 1.644237685604219790 ) ) ;
#7051 = DIRECTION ( 'NONE',  ( -0.08420877549337300871, 0.000000000000000000, -0.9964481331860212121 ) ) ;
#7050 = CARTESIAN_POINT ( 'NONE',  ( 1.179035820486476593, 11.63764180229748213, 6.543292337723209506 ) ) ;
#7052 = ORIENTED_EDGE ( 'NONE', *, *, #705, .F. ) ;
#7053 = CARTESIAN_POINT ( 'NONE',  ( 5.114825480111228728, 11.70051646708293269, 6.098904411201394815 ) ) ;
#7054 = ORIENTED_EDGE ( 'NONE', *, *, #8671, .F. ) ;
#7055 = CARTESIAN_POINT ( 'NONE',  ( 53.84486179190094646, 34.52875999999999834, -6.412645463410259872 ) ) ;
#7056 = ADVANCED_FACE ( 'NONE', ( #9394 ), #12726, .T. ) ;
#7057 = AXIS2_PLACEMENT_3D ( 'NONE', #1800, #10102, #11876 ) ;
#7058 = EDGE_LOOP ( 'NONE', ( #13050, #5269, #6602, #10827 ) ) ;
#7059 = EDGE_CURVE ( 'NONE', #1295, #4521, #15583, .T. ) ;
#7060 = CARTESIAN_POINT ( 'NONE',  ( 7.752716165273062288, 18.41075878025652557, -1.699111224125438024 ) ) ;
#7061 = DIRECTION ( 'NONE',  ( -0.08192867786951699149, 0.000000000000000000, -0.9966381950048638361 ) ) ;
#7062 = VERTEX_POINT ( 'NONE', #988 ) ;
#7063 = AXIS2_PLACEMENT_3D ( 'NONE', #4452, #21343, #19680 ) ;
#7064 = DIRECTION ( 'NONE',  ( 0.000000000000000000, 1.000000000000000000, 0.000000000000000000 ) ) ;
#7065 = DIRECTION ( 'NONE',  ( 0.000000000000000000, 1.000000000000000000, 0.000000000000000000 ) ) ;
#7066 = DIRECTION ( 'NONE',  ( 1.000000000000000000, 0.000000000000000000, 0.000000000000000000 ) ) ;
#7067 = CARTESIAN_POINT ( 'NONE',  ( 2.112882994232062828, 21.07822518102817000, 5.653028666727347940 ) ) ;
#7068 = DIRECTION ( 'NONE',  ( 0.2490110332224857170, 0.000000000000000000, -0.9685006480810790519 ) ) ;
#7069 = AXIS2_PLACEMENT_3D ( 'NONE', #20332, #15080, #11518 ) ;
#7070 = VERTEX_POINT ( 'NONE', #19450 ) ;
#7071 = CARTESIAN_POINT ( 'NONE',  ( 1.011698528169785005, 19.61962022855508181, 7.364809558829694680 ) ) ;
#7072 = DIRECTION ( 'NONE',  ( 0.1060008583745224581, 0.000000000000000000, 0.9943660382494288186 ) ) ;
#7073 = FACE_OUTER_BOUND ( 'NONE', #4841, .T. ) ;
#7074 = EDGE_CURVE ( 'NONE', #15662, #4928, #14531, .T. ) ;
#7075 = DIRECTION ( 'NONE',  ( -0.2490110332224848011, 0.000000000000000000, 0.9685006480810792739 ) ) ;
#7076 = ORIENTED_EDGE ( 'NONE', *, *, #12544, .T. ) ;
#7077 = CARTESIAN_POINT ( 'NONE',  ( 10.47598215385642639, 10.97943152176106274, 4.232648866062586279 ) ) ;
#7078 = CIRCLE ( 'NONE', #7063, 0.5080000000000000071 ) ;
#7079 = FACE_OUTER_BOUND ( 'NONE', #15007, .T. ) ;
#7080 = CARTESIAN_POINT ( 'NONE',  ( 12.60809324200862314, 20.43343092864591881, 5.533879428115382026 ) ) ;
#7081 = ORIENTED_EDGE ( 'NONE', *, *, #13591, .T. ) ;
#7082 = CIRCLE ( 'NONE', #14867, 0.5079999999999984528 ) ;
#7083 = ORIENTED_EDGE ( 'NONE', *, *, #19281, .T. ) ;
#7084 = LINE ( 'NONE', #12066, #4602 ) ;
#7085 = CARTESIAN_POINT ( 'NONE',  ( 9.182002370748412190, 12.08590500130187628, 6.093407161457568222 ) ) ;
#7086 = CARTESIAN_POINT ( 'NONE',  ( 7.082014623697716615, 18.17920521194865913, 7.349654649369399273 ) ) ;
#7087 = DIRECTION ( 'NONE',  ( 1.000000000000000000, 0.000000000000000000, 0.000000000000000000 ) ) ;
#7088 = EDGE_CURVE ( 'NONE', #10693, #2731, #10842, .T. ) ;
#7089 = CARTESIAN_POINT ( 'NONE',  ( 5.588162325894102445, 14.98248962140982599, -1.190334577872725230 ) ) ;
#7090 = CIRCLE ( 'NONE', #11343, 9.525000000000000355 ) ;
#7091 = DIRECTION ( 'NONE',  ( 0.05085730733808139364, 0.000000000000000000, -0.9987059298363658577 ) ) ;
#7092 = EDGE_CURVE ( 'NONE', #20045, #8589, #16060, .T. ) ;
#7093 = CARTESIAN_POINT ( 'NONE',  ( 30.42699695299585017, -3.968114999999999615, -4.832012189960551041 ) ) ;
#7094 = CARTESIAN_POINT ( 'NONE',  ( 11.65780787164172594, 18.24951553479433031, -3.906928721014021555 ) ) ;
#7095 = CARTESIAN_POINT ( 'NONE',  ( 5.184282268542144578, 13.02144258489116702, 6.600906927883145592 ) ) ;
#7096 = VECTOR ( 'NONE', #15195, 1000.000000000000227 ) ;
#7097 = DIRECTION ( 'NONE',  ( 0.4987171968201936645, 0.000000000000000000, -0.8667647648559603235 ) ) ;
#7098 = CARTESIAN_POINT ( 'NONE',  ( 2.170325927336617777, 11.82982598436980126, 1.730999371418365129 ) ) ;
#7099 = CARTESIAN_POINT ( 'NONE',  ( 0.8193983463107750165, 20.11811364056184459, 7.806734921283819517 ) ) ;
#7100 = DIRECTION ( 'NONE',  ( -0.000000000000000000, -1.000000000000000000, 0.000000000000000000 ) ) ;
#7101 = CARTESIAN_POINT ( 'NONE',  ( 3.987335596668034388, 20.53326216353070421, 5.068335100042532737 ) ) ;
#7102 = CARTESIAN_POINT ( 'NONE',  ( 7.735533989518945219, 6.343967500000000648, -21.17236077523805449 ) ) ;
#7103 = DIRECTION ( 'NONE',  ( -1.000000000000000000, 0.000000000000000000, 0.000000000000000000 ) ) ;
#7104 = CARTESIAN_POINT ( 'NONE',  ( 13.29287104629461780, -7.674283192410473298, -16.66854283075998566 ) ) ;
#7105 = ADVANCED_FACE ( 'NONE', ( #892 ), #21218, .T. ) ;
#7106 = AXIS2_PLACEMENT_3D ( 'NONE', #5791, #12550, #18169 ) ;
#7107 = EDGE_CURVE ( 'NONE', #9848, #12344, #3911, .T. ) ;
#7108 = DIRECTION ( 'NONE',  ( 0.9636276526537417286, 0.000000000000000000, -0.2672484743474500268 ) ) ;
#7109 = CIRCLE ( 'NONE', #13829, 1.983739999999997838 ) ;
#7110 = DIRECTION ( 'NONE',  ( -0.1060008583745200572, 0.000000000000000000, -0.9943660382494290406 ) ) ;
#7111 = CARTESIAN_POINT ( 'NONE',  ( 11.44031352510691946, 15.54975579857636880, 7.527537594959339273 ) ) ;
#7112 = DIRECTION ( 'NONE',  ( 0.4857267349359797870, 0.000000000000000000, -0.8741107132214044340 ) ) ;
#7113 = AXIS2_PLACEMENT_3D ( 'NONE', #10614, #12172, #17248 ) ;
#7114 = CARTESIAN_POINT ( 'NONE',  ( 12.32163425866073148, 11.24196547682344161, 2.114862982211144438 ) ) ;
#7115 = DIRECTION ( 'NONE',  ( 0.000000000000000000, 1.000000000000000000, 0.000000000000000000 ) ) ;
#7116 = CARTESIAN_POINT ( 'NONE',  ( 6.969861975853656411, 13.41850193825106174, 6.940434113064578803 ) ) ;
#7117 = EDGE_LOOP ( 'NONE', ( #7390, #9991, #3172, #8539 ) ) ;
#7118 = SHAPE_DEFINITION_REPRESENTATION ( #14143, #13411 ) ;
#7119 = VECTOR ( 'NONE', #20197, 1000.000000000000000 ) ;
#7120 = CARTESIAN_POINT ( 'NONE',  ( 0.2363768735086284323, 20.63358941134637092, 5.024770624937192842 ) ) ;
#7121 = DIRECTION ( 'NONE',  ( 1.000000000000000000, 0.000000000000000000, 0.000000000000000000 ) ) ;
#7122 = DIRECTION ( 'NONE',  ( -0.7421532822901562021, 0.000000000000000000, 0.6702301885068651099 ) ) ;
#7123 = VECTOR ( 'NONE', #20657, 1000.000000000000000 ) ;
#7124 = AXIS2_PLACEMENT_3D ( 'NONE', #12512, #18017, #4099 ) ;
#7125 = CARTESIAN_POINT ( 'NONE',  ( 14.72818571777967911, -8.530828868335872173, -15.61771171534634917 ) ) ;
#7126 = ORIENTED_EDGE ( 'NONE', *, *, #2516, .F. ) ;
#7127 = CARTESIAN_POINT ( 'NONE',  ( 7.744502704386849068, 18.07137575567074350, -1.961665155297699137 ) ) ;
#7128 = CARTESIAN_POINT ( 'NONE',  ( 4.355808376242262803, 20.06831615587024586, 5.938053330416548370 ) ) ;
#7129 = CARTESIAN_POINT ( 'NONE',  ( 5.988546274437528183, 18.80336625489407965, -0.8540819367508141191 ) ) ;
#7130 = CARTESIAN_POINT ( 'NONE',  ( 7.492294575654238287, 12.00122113815488056, 5.673272314834056473 ) ) ;
#7131 = CARTESIAN_POINT ( 'NONE',  ( 9.028821228240033747, 11.50047795576720233, 5.514895994043016891 ) ) ;
#7132 = AXIS2_PLACEMENT_3D ( 'NONE', #3653, #13838, #17141 ) ;
#7133 = B_SPLINE_CURVE_WITH_KNOTS ( 'NONE', 3,
 ( #20970, #9459, #12580, #7698, #11127 ),
 .UNSPECIFIED., .F., .F.,
 ( 4, 1, 4 ),
 ( 0.000000000000000000, 0.2499992869893835068, 0.4992858149431267933 ),
 .UNSPECIFIED. ) ;
#7134 = DIRECTION ( 'NONE',  ( 0.000000000000000000, -1.000000000000000000, 0.000000000000000000 ) ) ;
#7135 = CARTESIAN_POINT ( 'NONE',  ( 12.56202611117371681, -0.7075020235198306029, -16.53645491934344136 ) ) ;
#7136 = ADVANCED_FACE ( 'NONE', ( #6192 ), #19667, .T. ) ;
#7137 = DIRECTION ( 'NONE',  ( -0.2868778675745011220, 0.000000000000000000, -0.9579671649362034858 ) ) ;
#7138 = ORIENTED_EDGE ( 'NONE', *, *, #17673, .F. ) ;
#7139 = CARTESIAN_POINT ( 'NONE',  ( 11.16823954825894205, 13.89705342359357054, 6.200388406566677446 ) ) ;
#7140 = CARTESIAN_POINT ( 'NONE',  ( 5.792514709454430921, 19.23872087217396398, -1.508687341247886948 ) ) ;
#7141 = AXIS2_PLACEMENT_3D ( 'NONE', #21645, #19647, #6057 ) ;
#7142 = VERTEX_POINT ( 'NONE', #16378 ) ;
#7143 = VECTOR ( 'NONE', #10142, 1000.000000000000000 ) ;
#7144 = CARTESIAN_POINT ( 'NONE',  ( 10.28716446386076555, 11.36762743660578145, 2.108319987653204830 ) ) ;
#7145 = DIRECTION ( 'NONE',  ( 0.9790635044817341814, 0.000000000000000000, -0.2035550397114870014 ) ) ;
#7146 = LINE ( 'NONE', #13912, #3976 ) ;
#7148 = LINE ( 'NONE', #15230, #16299 ) ;
#7147 = CARTESIAN_POINT ( 'NONE',  ( 4.701992403669415843, 11.43043024698558163, 5.679938558605459598 ) ) ;
#7149 = ORIENTED_EDGE ( 'NONE', *, *, #15032, .T. ) ;
#7150 = CARTESIAN_POINT ( 'NONE',  ( 7.494300422474976742, 13.81960511660041746, 7.795597158064130561 ) ) ;
#7151 = AXIS2_PLACEMENT_3D ( 'NONE', #3408, #11816, #13375 ) ;
#7152 = DIRECTION ( 'NONE',  ( -0.9685006480810792739, 0.000000000000000000, -0.2490110332224846346 ) ) ;
#7153 = ORIENTED_EDGE ( 'NONE', *, *, #18805, .F. ) ;
#7154 = AXIS2_PLACEMENT_3D ( 'NONE', #18068, #9542, #14665 ) ;
#7155 = DIRECTION ( 'NONE',  ( -0.000000000000000000, -1.000000000000000000, 0.000000000000000000 ) ) ;
#7156 = ORIENTED_EDGE ( 'NONE', *, *, #21877, .F. ) ;
#7157 = CYLINDRICAL_SURFACE ( 'NONE', #1146, 0.5079999999999965654 ) ;
#7158 = CARTESIAN_POINT ( 'NONE',  ( 1.933308127472557647, 14.06219242987879703, 0.7237907644290267895 ) ) ;
#7159 = AXIS2_PLACEMENT_3D ( 'NONE', #3181, #20391, #8584 ) ;
#7160 = CARTESIAN_POINT ( 'NONE',  ( 38.82016491058538321, 42.06303499999999929, -14.75770094105646812 ) ) ;
#7161 = CARTESIAN_POINT ( 'NONE',  ( 12.11879977990919421, 13.08893749999999834, 0.1373704394269426865 ) ) ;
#7162 = CARTESIAN_POINT ( 'NONE',  ( 42.35466991749225940, 42.06303499999999929, -17.94967221382040279 ) ) ;
#7163 = EDGE_CURVE ( 'NONE', #20627, #18152, #7412, .T. ) ;
#7164 = DIRECTION ( 'NONE',  ( -0.6702301885068628895, 0.000000000000000000, -0.7421532822901579785 ) ) ;
#7165 = AXIS2_PLACEMENT_3D ( 'NONE', #4635, #2654, #19558 ) ;
#7166 = EDGE_LOOP ( 'NONE', ( #14920, #7153, #55, #13922 ) ) ;
#7167 = LINE ( 'NONE', #14258, #3646 ) ;
#7168 = DIRECTION ( 'NONE',  ( -0.2490110332224846346, 0.000000000000000000, 0.9685006480810792739 ) ) ;
#7170 = CARTESIAN_POINT ( 'NONE',  ( 18.39572628222328277, -6.194563955895442398, -14.37377832747673168 ) ) ;
#7169 = DIRECTION ( 'NONE',  ( -0.5087559856598092844, 0.000000000000000000, -0.8609107660235849613 ) ) ;
#7171 = VERTEX_POINT ( 'NONE', #9822 ) ;
#7172 = VERTEX_POINT ( 'NONE', #9936 ) ;
#7173 = CARTESIAN_POINT ( 'NONE',  ( 12.98496071183864586, 13.22236995718078134, 5.543149843602365401 ) ) ;
#7175 = DIRECTION ( 'NONE',  ( 0.9685006480810792739, 0.000000000000000000, 0.2490110332224850509 ) ) ;
#7174 = CARTESIAN_POINT ( 'NONE',  ( 5.603942890132661780, 13.84493627167355179, 8.299647925973943074 ) ) ;
#7176 = VERTEX_POINT ( 'NONE', #11828 ) ;
#7178 = CARTESIAN_POINT ( 'NONE',  ( 11.41584562260435476, -6.408040714559842144, -16.92812135191189071 ) ) ;
#7177 = CARTESIAN_POINT ( 'NONE',  ( 4.319597228044323778, 11.18970892858293276, 2.675083765875428732 ) ) ;
#7179 = CIRCLE ( 'NONE', #1513, 4.365624999999999645 ) ;
#7180 = ORIENTED_EDGE ( 'NONE', *, *, #14570, .T. ) ;
#7181 = VERTEX_POINT ( 'NONE', #16590 ) ;
#7182 = CARTESIAN_POINT ( 'NONE',  ( 7.573246980053331967, 17.33572519892136654, -2.036030731767461521 ) ) ;
#7183 = AXIS2_PLACEMENT_3D ( 'NONE', #16736, #4891, #243 ) ;
#7184 = ORIENTED_EDGE ( 'NONE', *, *, #5921, .T. ) ;
#7185 = CARTESIAN_POINT ( 'NONE',  ( 3.427325199255271126, 15.53052183636367722, 8.374923869955427591 ) ) ;
#7186 = DIRECTION ( 'NONE',  ( 0.000000000000000000, 1.000000000000000000, 0.000000000000000000 ) ) ;
#7187 = CARTESIAN_POINT ( 'NONE',  ( 1.581041518826207248, 34.52875999999999834, -20.30277549736237575 ) ) ;
#7188 = AXIS2_PLACEMENT_3D ( 'NONE', #9244, #16027, #6038 ) ;
#7189 = CARTESIAN_POINT ( 'NONE',  ( 38.73876173903332898, -7.523800691136061758, -4.196965627914218899 ) ) ;
#7190 = CARTESIAN_POINT ( 'NONE',  ( 39.27728671717661513, 32.54502000000000095, -23.95520057284206672 ) ) ;
#7191 = LINE ( 'NONE', #649, #8629 ) ;
#7192 = CARTESIAN_POINT ( 'NONE',  ( 1.254300738082038125, 21.01230615663556023, 3.340964865855025945 ) ) ;
#7193 = EDGE_CURVE ( 'NONE', #13038, #395, #7961, .T. ) ;
#7194 = FACE_BOUND ( 'NONE', #11474, .T. ) ;
#7195 = EDGE_CURVE ( 'NONE', #12892, #13849, #729, .T. ) ;
#7196 = ORIENTED_EDGE ( 'NONE', *, *, #16138, .T. ) ;
#7197 = CARTESIAN_POINT ( 'NONE',  ( 0.5413756995750967915, 12.83134191367328292, 1.794410497042580266 ) ) ;
#7198 = CARTESIAN_POINT ( 'NONE',  ( 39.42154620619601957, -6.356984999999999886, -4.343957374021048423 ) ) ;
#7199 = CARTESIAN_POINT ( 'NONE',  ( 53.83440531914143179, -5.732648258448109324, -15.79034767386256988 ) ) ;
#7200 = DIRECTION ( 'NONE',  ( 0.000000000000000000, 0.000000000000000000, 1.000000000000000000 ) ) ;
#7201 = ORIENTED_EDGE ( 'NONE', *, *, #2950, .T. ) ;
#7202 = ORIENTED_EDGE ( 'NONE', *, *, #2738, .T. ) ;
#7203 = CARTESIAN_POINT ( 'NONE',  ( 10.89469307076425686, 21.76139788190002022, 2.134525428084244947 ) ) ;
#7204 = AXIS2_PLACEMENT_3D ( 'NONE', #3235, #1458, #16616 ) ;
#7205 = CARTESIAN_POINT ( 'NONE',  ( 29.76562500000000000, 32.54502000000000095, -4.317999999999999616 ) ) ;
#7206 = CARTESIAN_POINT ( 'NONE',  ( 13.14944941967905301, 12.29607346375136068, 5.638298986518227807 ) ) ;
#7207 = ORIENTED_EDGE ( 'NONE', *, *, #18883, .F. ) ;
#7208 = ORIENTED_EDGE ( 'NONE', *, *, #20067, .T. ) ;
#7209 = DIRECTION ( 'NONE',  ( -0.7421532822901579785, 0.000000000000000000, 0.6702301885068630005 ) ) ;
#7210 = CARTESIAN_POINT ( 'NONE',  ( 9.015524272356790547, 11.53921692834158286, 5.350368841146013743 ) ) ;
#7211 = CARTESIAN_POINT ( 'NONE',  ( 0.7257397583488034432, 19.54979116365418079, 7.396820614257542559 ) ) ;
#7212 = CARTESIAN_POINT ( 'NONE',  ( 64.14292646034530776, 32.54502000000000095, -12.24881465648521939 ) ) ;
#7213 = CARTESIAN_POINT ( 'NONE',  ( 5.929260172323883360, 18.48292898978692023, -0.9131295676930929472 ) ) ;
#7214 = AXIS2_PLACEMENT_3D ( 'NONE', #13720, #1435, #18778 ) ;
#7215 = CARTESIAN_POINT ( 'NONE',  ( 1.508768852107567504, 20.36732049711449832, 4.044819003516886724 ) ) ;
#7216 = CARTESIAN_POINT ( 'NONE',  ( 59.80894853325292360, -6.356984999999999886, -16.70545285374888778 ) ) ;
#7217 = EDGE_CURVE ( 'NONE', #19328, #6310, #16698, .T. ) ;
#7218 = CARTESIAN_POINT ( 'NONE',  ( 39.62791084302666178, -1.983739999999999837, -24.65774797299118859 ) ) ;
#7219 = CARTESIAN_POINT ( 'NONE',  ( 11.74500383039051776, 15.67423727725497606, 7.485740281064174440 ) ) ;
#7220 = CARTESIAN_POINT ( 'NONE',  ( 5.068394031931605426, 12.56749199890325208, 6.028102843334117722 ) ) ;
#7221 = VECTOR ( 'NONE', #20537, 1000.000000000000000 ) ;
#7222 = CARTESIAN_POINT ( 'NONE',  ( 5.075711589750377506, 21.42306324396562189, 1.964058843707486179 ) ) ;
#7223 = CARTESIAN_POINT ( 'NONE',  ( 1.469492836360677179, 17.96208015702665861, 9.343845014913002345 ) ) ;
#7224 = EDGE_CURVE ( 'NONE', #12892, #19746, #21662, .T. ) ;
#7225 = EDGE_CURVE ( 'NONE', #10798, #12065, #1639, .T. ) ;
#7226 = LINE ( 'NONE', #8857, #3988 ) ;
#7227 = CARTESIAN_POINT ( 'NONE',  ( 6.282630550826245219, 11.65589518700730132, 2.475056272112619027 ) ) ;
#7228 = DIRECTION ( 'NONE',  ( 0.000000000000000000, 1.000000000000000000, 0.000000000000000000 ) ) ;
#7229 = DIRECTION ( 'NONE',  ( 0.2490110332224850509, 0.000000000000000000, -0.9685006480810792739 ) ) ;
#7230 = CARTESIAN_POINT ( 'NONE',  ( 19.00809320208830044, 1.143335664616400571, -14.55959509790053730 ) ) ;
#7231 = CIRCLE ( 'NONE', #19574, 6.350000000000002309 ) ;
#7232 = DIRECTION ( 'NONE',  ( 0.000000000000000000, -1.000000000000000000, -0.000000000000000000 ) ) ;
#7233 = CARTESIAN_POINT ( 'NONE',  ( 11.29708385613510657, 17.57508648399901574, 7.446457121411568458 ) ) ;
#7234 = ORIENTED_EDGE ( 'NONE', *, *, #7432, .F. ) ;
#7235 = CARTESIAN_POINT ( 'NONE',  ( -2.845411283647486300, -0.7997824999999986195, -5.196881601526627925 ) ) ;
#7236 = CARTESIAN_POINT ( 'NONE',  ( 11.96961372335506901, 11.26714859802527080, 0.6016620342287901657 ) ) ;
#7237 = CARTESIAN_POINT ( 'NONE',  ( 12.53629344102889043, -6.118443352698756499, -15.63122047053925812 ) ) ;
#7238 = VECTOR ( 'NONE', #1486, 1000.000000000000227 ) ;
#7239 = ORIENTED_EDGE ( 'NONE', *, *, #16189, .T. ) ;
#7240 = CARTESIAN_POINT ( 'NONE',  ( 11.42842559562532578, 34.52875999999999834, 1.673196738795719174 ) ) ;
#7241 = FACE_OUTER_BOUND ( 'NONE', #16232, .T. ) ;
#7242 = EDGE_CURVE ( 'NONE', #7810, #21532, #21437, .T. ) ;
#7243 = VECTOR ( 'NONE', #18564, 1000.000000000000114 ) ;
#7244 = PRODUCT_DEFINITION_SHAPE ( 'NONE', 'NONE',  #21885 ) ;
#7245 = EDGE_LOOP ( 'NONE', ( #2192, #15565, #2815, #7023, #9253, #6289, #13673, #20826 ) ) ;
#7246 = CARTESIAN_POINT ( 'NONE',  ( 6.809079960824258038, 11.82958596167992127, 4.252032552716304536 ) ) ;
#7247 = CARTESIAN_POINT ( 'NONE',  ( 12.49792962410951525, 19.94285714604490067, 5.068850365372612465 ) ) ;
#7248 = CARTESIAN_POINT ( 'NONE',  ( 1.957605007174791467, 13.96208391574584162, 8.945319323778717191 ) ) ;
#7249 = CARTESIAN_POINT ( 'NONE',  ( 11.47115874364255994, 10.98707485392928085, -1.321792392077711487 ) ) ;
#7250 = DIRECTION ( 'NONE',  ( -0.2490110332224836354, 0.000000000000000000, 0.9685006480810794960 ) ) ;
#7251 = ORIENTED_EDGE ( 'NONE', *, *, #19539, .F. ) ;
#7252 = CARTESIAN_POINT ( 'NONE',  ( 11.06571474200560345, 17.46349345829840161, 6.690722436210692514 ) ) ;
#7253 = CARTESIAN_POINT ( 'NONE',  ( 7.233972636490444863, 16.38025891712375781, -3.007816387549334003 ) ) ;
#7254 = CYLINDRICAL_SURFACE ( 'NONE', #8089, 0.7950200000000000600 ) ;
#7255 = AXIS2_PLACEMENT_3D ( 'NONE', #9377, #1200, #19553 ) ;
#7256 = EDGE_LOOP ( 'NONE', ( #16025, #15491, #16691, #4411, #9777, #6695 ) ) ;
#7257 = CARTESIAN_POINT ( 'NONE',  ( 9.677015374421488403, 12.13265719289923616, -0.5781317187935294255 ) ) ;
#7258 = CARTESIAN_POINT ( 'NONE',  ( -15.27935546639805331, 38.49687500000000284, -26.04713531390440906 ) ) ;
#7259 = CARTESIAN_POINT ( 'NONE',  ( -17.46249999999999858, -1.983740000000001169, 0.000000000000000000 ) ) ;
#7261 = DIRECTION ( 'NONE',  ( 0.000000000000000000, -1.000000000000000000, -0.000000000000000000 ) ) ;
#7260 = CARTESIAN_POINT ( 'NONE',  ( -1.007450280090600003, 20.72700438578640458, 3.842530817846650848 ) ) ;
#7262 = ORIENTED_EDGE ( 'NONE', *, *, #15391, .T. ) ;
#7263 = ORIENTED_EDGE ( 'NONE', *, *, #18069, .F. ) ;
#7264 = DIRECTION ( 'NONE',  ( 0.9685006480810792739, -0.000000000000000000, 0.2490110332224850509 ) ) ;
#7265 = EDGE_CURVE ( 'NONE', #9462, #777, #6407, .T. ) ;
#7266 = ADVANCED_FACE ( 'NONE', ( #11603 ), #2996, .F. ) ;
#7267 = CARTESIAN_POINT ( 'NONE',  ( 12.44431693874740041, -5.663843069250676265, -16.77216482461518865 ) ) ;
#7268 = VERTEX_POINT ( 'NONE', #6730 ) ;
#7269 = CARTESIAN_POINT ( 'NONE',  ( -4.728951812473551897, 2.373947500000000765, -29.02782796843600011 ) ) ;
#7270 = PLANE ( 'NONE',  #3278 ) ;
#7271 = FACE_OUTER_BOUND ( 'NONE', #19724, .T. ) ;
#7272 = DIRECTION ( 'NONE',  ( 0.000000000000000000, -1.000000000000000000, -0.000000000000000000 ) ) ;
#7273 = ORIENTED_EDGE ( 'NONE', *, *, #5736, .F. ) ;
#7274 = CARTESIAN_POINT ( 'NONE',  ( 8.011380105705496746, -6.752907499999998286, -19.05252355006962617 ) ) ;
#7275 = CARTESIAN_POINT ( 'NONE',  ( -15.39353573898878658, 34.79968030885680008, -10.30107656633069979 ) ) ;
#7276 = CARTESIAN_POINT ( 'NONE',  ( 20.50345441762315346, -0.2404631712157635770, -15.38884510733137567 ) ) ;
#7278 = CARTESIAN_POINT ( 'NONE',  ( 19.66680293064437279, -4.114175158726030013, -14.16347315398008888 ) ) ;
#7277 = DIRECTION ( 'NONE',  ( 0.000000000000000000, 1.000000000000000000, 0.000000000000000000 ) ) ;
#7279 = VERTEX_POINT ( 'NONE', #13176 ) ;
#7280 = ORIENTED_EDGE ( 'NONE', *, *, #11801, .F. ) ;
#7281 = CARTESIAN_POINT ( 'NONE',  ( 11.51858435347932108, 11.70279650494946289, -0.9316420090841365242 ) ) ;
#7282 = CARTESIAN_POINT ( 'NONE',  ( 7.549769109252762789, 16.64380874522678155, 8.484748712165586682 ) ) ;
#7283 = VERTEX_POINT ( 'NONE', #18558 ) ;
#7285 = CARTESIAN_POINT ( 'NONE',  ( 11.35372246689305875, 0.1808204478124068870, -16.88120184474271213 ) ) ;
#7284 = CARTESIAN_POINT ( 'NONE',  ( 4.161695538953418705, 11.38564755976896237, 1.994139648140534904 ) ) ;
#7286 = VERTEX_POINT ( 'NONE', #15055 ) ;
#7287 = EDGE_LOOP ( 'NONE', ( #17893, #16910, #11273, #17341, #9871 ) ) ;
#7288 = CARTESIAN_POINT ( 'NONE',  ( 7.685683886033650047, 12.68839834003130740, -0.4749676218993871823 ) ) ;
#7289 = ADVANCED_FACE ( 'NONE', ( #3419 ), #18339, .F. ) ;
#7290 = ORIENTED_EDGE ( 'NONE', *, *, #17344, .F. ) ;
#7291 = CARTESIAN_POINT ( 'NONE',  ( 15.58268548097005102, 0.3514302678472279728, 9.860356909081639643 ) ) ;
#7292 = CARTESIAN_POINT ( 'NONE',  ( 66.03921914090641110, 30.56064500000000095, -10.93409647675949969 ) ) ;
#7293 = CARTESIAN_POINT ( 'NONE',  ( 36.51250000000000284, 0.000000000000000000, -10.31875000000000142 ) ) ;
#7294 = CARTESIAN_POINT ( 'NONE',  ( 2.579465434524714329, 20.56131833015633248, 6.894018011111492150 ) ) ;
#7295 = CARTESIAN_POINT ( 'NONE',  ( -13.87568970999206108, -1.983739999999999393, -9.457638332870221376 ) ) ;
#7296 = ORIENTED_EDGE ( 'NONE', *, *, #3028, .T. ) ;
#7297 = CARTESIAN_POINT ( 'NONE',  ( 4.811918810904475485, 19.96663567226219982, 0.7225885738512296541 ) ) ;
#7298 = CARTESIAN_POINT ( 'NONE',  ( 64.14292646034530776, 34.52875999999999834, -12.24881465648521939 ) ) ;
#7299 = LINE ( 'NONE', #19229, #18772 ) ;
#7300 = CYLINDRICAL_SURFACE ( 'NONE', #7831, 9.524999999999996803 ) ;
#7301 = ORIENTED_EDGE ( 'NONE', *, *, #15721, .F. ) ;
#7302 = EDGE_LOOP ( 'NONE', ( #11056, #12267, #9229, #11291 ) ) ;
#7303 = CARTESIAN_POINT ( 'NONE',  ( 9.334271081287811356, 21.44638057025442279, 3.630935037030034618 ) ) ;
#7304 = AXIS2_PLACEMENT_3D ( 'NONE', #12511, #774, #12721 ) ;
#7305 = DIRECTION ( 'NONE',  ( 0.9564948366894089338, 0.05542109139015086172, -0.2864369564417716951 ) ) ;
#7306 = CARTESIAN_POINT ( 'NONE',  ( 11.56023901238583207, 10.99603790901469225, -1.079658926462704560 ) ) ;
#7307 = ORIENTED_EDGE ( 'NONE', *, *, #11423, .F. ) ;
#7308 = ORIENTED_EDGE ( 'NONE', *, *, #15817, .T. ) ;
#7309 = DIRECTION ( 'NONE',  ( -0.5171931484643310650, -0.000000000000000000, -0.8558687090795833452 ) ) ;
#7310 = CARTESIAN_POINT ( 'NONE',  ( 7.235594381361154959, 14.41299800172950185, -2.541178202713186618 ) ) ;
#7311 = CARTESIAN_POINT ( 'NONE',  ( 6.005363321636888685, 12.27588422369934129, 0.9603231873459451284 ) ) ;
#7312 = CARTESIAN_POINT ( 'NONE',  ( 57.35354854712898742, 0.000000000000000000, -21.22263945788050776 ) ) ;
#7313 = CARTESIAN_POINT ( 'NONE',  ( 6.035915765164218350, 18.90302373985587536, -0.6745700400264159624 ) ) ;
#7314 = CARTESIAN_POINT ( 'NONE',  ( 7.303925134678800113, 14.37207998726623615, 7.210427461397269866 ) ) ;
#7315 = EDGE_CURVE ( 'NONE', #1762, #5667, #15153, .T. ) ;
#7316 = DIRECTION ( 'NONE',  ( 0.08420877549337300871, 0.000000000000000000, 0.9964481331860212121 ) ) ;
#7317 = CARTESIAN_POINT ( 'NONE',  ( 14.05820270259704152, 128.5105379999999968, -15.03781736451272444 ) ) ;
#7318 = AXIS2_PLACEMENT_3D ( 'NONE', #6286, #16694, #9931 ) ;
#7319 = CARTESIAN_POINT ( 'NONE',  ( 8.033113057174002591, 11.41928500448566375, -0.1748968685806625845 ) ) ;
#7320 = FACE_OUTER_BOUND ( 'NONE', #14560, .T. ) ;
#7321 = FACE_OUTER_BOUND ( 'NONE', #9418, .T. ) ;
#7322 = FACE_OUTER_BOUND ( 'NONE', #1594, .T. ) ;
#7323 = CYLINDRICAL_SURFACE ( 'NONE', #16706, 0.3962399999999975386 ) ;
#7324 = CARTESIAN_POINT ( 'NONE',  ( 1.078174312258882273, 18.49964734577863368, 8.341151507176290281 ) ) ;
#7325 = DIRECTION ( 'NONE',  ( 0.000000000000000000, -1.000000000000000000, 0.000000000000000000 ) ) ;
#7326 = FACE_OUTER_BOUND ( 'NONE', #5501, .T. ) ;
#7327 = CARTESIAN_POINT ( 'NONE',  ( 20.31958935979195857, -0.4446614350344761935, -14.14521446648425851 ) ) ;
#7328 = DIRECTION ( 'NONE',  ( 0.000000000000000000, 1.000000000000000000, 0.000000000000000000 ) ) ;
#7329 = CARTESIAN_POINT ( 'NONE',  ( 11.41150532678066476, 14.07074566132039095, 7.133435626371687377 ) ) ;
#7330 = ORIENTED_EDGE ( 'NONE', *, *, #212, .T. ) ;
#7331 = ADVANCED_FACE ( 'NONE', ( #14948 ), #3098, .F. ) ;
#7332 = DIRECTION ( 'NONE',  ( -0.3140771401027084853, 0.9459569826691583971, -0.08075231887918270235 ) ) ;
#7333 = CARTESIAN_POINT ( 'NONE',  ( 11.69498266538699838, 11.63108941959115050, -0.5923512581102406971 ) ) ;
#7334 = DIRECTION ( 'NONE',  ( 0.000000000000000000, 1.000000000000000000, -0.000000000000000000 ) ) ;
#7335 = VERTEX_POINT ( 'NONE', #19771 ) ;
#7336 = PRODUCT_CONTEXT ( 'NONE', #13863, 'mechanical' ) ;
#7337 = CARTESIAN_POINT ( 'NONE',  ( 46.07940063401251507, 34.52875999999999834, -26.08707253294707229 ) ) ;
#7338 = ADVANCED_FACE ( 'NONE', ( #6618 ), #11392, .F. ) ;
#7339 =( BOUNDED_CURVE ( )  B_SPLINE_CURVE ( 3, ( #21880, #20211, #1645, #15061 ),
 .UNSPECIFIED., .F., .T. ) 
 B_SPLINE_CURVE_WITH_KNOTS ( ( 4, 4 ),
 ( 4.712388980383330761, 6.283185307179586232 ),
 .UNSPECIFIED. ) 
 CURVE ( )  GEOMETRIC_REPRESENTATION_ITEM ( )  RATIONAL_B_SPLINE_CURVE ( ( 1.000000000000000000, 0.8047378541240446381, 0.8047378541240446381, 1.000000000000000000 ) ) 
 REPRESENTATION_ITEM ( '' )  );
#7340 = EDGE_CURVE ( 'NONE', #12596, #14993, #9721, .T. ) ;
#7341 = DIRECTION ( 'NONE',  ( 0.9579671649362034858, 0.000000000000000000, -0.2868778675745011220 ) ) ;
#7342 = EDGE_LOOP ( 'NONE', ( #17459, #11821, #20408, #18887 ) ) ;
#7343 = CARTESIAN_POINT ( 'NONE',  ( 13.50039319234801383, 21.41212481752907948, 2.265780506769165203 ) ) ;
#7344 = CARTESIAN_POINT ( 'NONE',  ( 8.142896893452514107, 20.59481639511846041, 4.729431829690726730 ) ) ;
#7345 = DIRECTION ( 'NONE',  ( -0.8609107660235850723, 0.000000000000000000, 0.5087559856598092844 ) ) ;
#7346 = CIRCLE ( 'NONE', #13719, 6.349999999999999645 ) ;
#7347 = DIRECTION ( 'NONE',  ( -0.4080888115384288528, 0.000000000000000000, -0.9129422336036122632 ) ) ;
#7348 = CARTESIAN_POINT ( 'NONE',  ( 17.80163320068923838, 0.5619476608638845905, -14.89932917514400224 ) ) ;
#7349 = LINE ( 'NONE', #5900, #4622 ) ;
#7350 = ORIENTED_EDGE ( 'NONE', *, *, #19779, .F. ) ;
#7351 = CARTESIAN_POINT ( 'NONE',  ( 12.03751388135225042, 21.69121361356170397, 3.958262461564761914 ) ) ;
#7352 = EDGE_CURVE ( 'NONE', #9795, #3518, #2850, .T. ) ;
#7353 = CARTESIAN_POINT ( 'NONE',  ( 39.42154620619643879, -5.166360000000000063, -4.343957374020580353 ) ) ;
#7354 = VERTEX_POINT ( 'NONE', #4960 ) ;
#7355 = CARTESIAN_POINT ( 'NONE',  ( 9.294776336270766492, 15.47881463844799832, -2.777761849933970240 ) ) ;
#7356 = DIRECTION ( 'NONE',  ( 0.000000000000000000, -1.000000000000000000, -0.000000000000000000 ) ) ;
#7357 = CARTESIAN_POINT ( 'NONE',  ( 12.50057563193774790, 21.92868216252701075, -0.5501692431105187353 ) ) ;
#7359 = DIRECTION ( 'NONE',  ( 0.2868778675745011220, 0.000000000000000000, 0.9579671649362033747 ) ) ;
#7358 = CARTESIAN_POINT ( 'NONE',  ( 3.448783566482409135, 12.50969690204968288, 0.7605462683841421878 ) ) ;
#7360 = ORIENTED_EDGE ( 'NONE', *, *, #10159, .F. ) ;
#7361 = CARTESIAN_POINT ( 'NONE',  ( 7.523395346134158501, 14.27362971915975187, 7.995196924124165605 ) ) ;
#7362 = CARTESIAN_POINT ( 'NONE',  ( 1.874333784495441968, 8.854522058277447982, 8.730299172444558664 ) ) ;
#7363 = AXIS2_PLACEMENT_3D ( 'NONE', #15207, #5227, #10324 ) ;
#7364 = ORIENTED_EDGE ( 'NONE', *, *, #5593, .T. ) ;
#7365 = EDGE_CURVE ( 'NONE', #4077, #17862, #11715, .T. ) ;
#7366 = DIRECTION ( 'NONE',  ( -0.1831666983862943188, 0.000000000000000000, 0.9830818687180962190 ) ) ;
#7367 = CARTESIAN_POINT ( 'NONE',  ( 20.04522676934494640, -2.740773359176641666, -14.07817139380126292 ) ) ;
#7368 = ORIENTED_EDGE ( 'NONE', *, *, #597, .F. ) ;
#7369 = DIRECTION ( 'NONE',  ( 0.05085730733808139364, 0.000000000000000000, -0.9987059298363658577 ) ) ;
#7370 = LINE ( 'NONE', #12915, #2197 ) ;
#7371 = PLANE ( 'NONE',  #17029 ) ;
#7372 = AXIS2_PLACEMENT_3D ( 'NONE', #19440, #17691, #4314 ) ;
#7373 = EDGE_LOOP ( 'NONE', ( #15734, #14065, #21143, #5810 ) ) ;
#7374 = DIRECTION ( 'NONE',  ( 0.000000000000000000, 1.000000000000000000, 0.000000000000000000 ) ) ;
#7375 = DIRECTION ( 'NONE',  ( 0.000000000000000000, 1.000000000000000000, 0.000000000000000000 ) ) ;
#7376 = EDGE_CURVE ( 'NONE', #8589, #10232, #4276, .T. ) ;
#7377 = CARTESIAN_POINT ( 'NONE',  ( 14.18258613239171062, -8.464138069599565384, -16.53238645035581911 ) ) ;
#7379 = CARTESIAN_POINT ( 'NONE',  ( 70.64340948846358970, 1.984375000000000000, -10.93409647675949969 ) ) ;
#7378 = DIRECTION ( 'NONE',  ( 0.3850029901312932989, 0.000000000000000000, -0.9229153252546862252 ) ) ;
#7380 = VERTEX_POINT ( 'NONE', #11926 ) ;
#7381 = EDGE_CURVE ( 'NONE', #7442, #11658, #12675, .T. ) ;
#7382 = ORIENTED_EDGE ( 'NONE', *, *, #6255, .F. ) ;
#7383 = EDGE_CURVE ( 'NONE', #490, #6167, #8484, .T. ) ;
#7385 = CARTESIAN_POINT ( 'NONE',  ( -17.46249999999999858, 32.54247999999999763, 0.000000000000000000 ) ) ;
#7384 = CARTESIAN_POINT ( 'NONE',  ( 3.813066075967610047, 12.19982130767714246, 0.3790570318242228454 ) ) ;
#7386 = VERTEX_POINT ( 'NONE', #5816 ) ;
#7388 = CARTESIAN_POINT ( 'NONE',  ( 10.60440690384716156, -4.915117656754341979, -15.85244087925699930 ) ) ;
#7387 = CARTESIAN_POINT ( 'NONE',  ( 5.583684207161521584, 15.96835738058210019, 8.791436236743251698 ) ) ;
#7389 = VERTEX_POINT ( 'NONE', #9117 ) ;
#7390 = ORIENTED_EDGE ( 'NONE', *, *, #7769, .F. ) ;
#7391 = CIRCLE ( 'NONE', #18674, 0.5080000000000000071 ) ;
#7392 = ORIENTED_EDGE ( 'NONE', *, *, #20820, .F. ) ;
#7393 = AXIS2_PLACEMENT_3D ( 'NONE', #12003, #12336, #7145 ) ;
#7394 = DIRECTION ( 'NONE',  ( -0.2868778675745011220, 0.000000000000000000, -0.9579671649362034858 ) ) ;
#7395 = AXIS2_PLACEMENT_3D ( 'NONE', #19914, #19801, #4677 ) ;
#7396 = DIRECTION ( 'NONE',  ( 0.000000000000000000, -1.000000000000000000, -0.000000000000000000 ) ) ;
#7397 = DIRECTION ( 'NONE',  ( 0.2490110332224850509, 0.000000000000000000, -0.9685006480810792739 ) ) ;
#7398 = CARTESIAN_POINT ( 'NONE',  ( 3.138855641000511287, 19.23123867353615069, 8.310718164606276659 ) ) ;
#7399 = ORIENTED_EDGE ( 'NONE', *, *, #16959, .T. ) ;
#7400 = CARTESIAN_POINT ( 'NONE',  ( 11.27494694361443628, -4.667157449014243120, -16.43482124609427686 ) ) ;
#7401 = CARTESIAN_POINT ( 'NONE',  ( 13.15085279376319782, 22.07249463472189888, 2.009202999722684790 ) ) ;
#7402 = DIRECTION ( 'NONE',  ( 0.000000000000000000, 1.000000000000000000, 0.000000000000000000 ) ) ;
#7403 = ORIENTED_EDGE ( 'NONE', *, *, #12212, .T. ) ;
#7404 = EDGE_CURVE ( 'NONE', #1876, #1202, #2389, .T. ) ;
#7405 = ORIENTED_EDGE ( 'NONE', *, *, #13057, .T. ) ;
#7406 = CARTESIAN_POINT ( 'NONE',  ( 11.55191247057558890, 21.31987603492770234, 3.934633224169304722 ) ) ;
#7408 = DIRECTION ( 'NONE',  ( -0.9579671649362032637, 0.000000000000000000, 0.2868778675745010664 ) ) ;
#7407 = DIRECTION ( 'NONE',  ( 0.000000000000000000, 1.000000000000000000, 0.000000000000000000 ) ) ;
#7409 = CARTESIAN_POINT ( 'NONE',  ( 11.23781920621831176, 11.97727348665198299, -2.482949163614870169 ) ) ;
#7410 = ORIENTED_EDGE ( 'NONE', *, *, #15903, .F. ) ;
#7411 = ORIENTED_EDGE ( 'NONE', *, *, #21537, .T. ) ;
#7412 = LINE ( 'NONE', #8062, #21555 ) ;
#7413 = CARTESIAN_POINT ( 'NONE',  ( 7.709748992265566869, 19.45393663054224831, -2.000501698392521455 ) ) ;
#7414 = CARTESIAN_POINT ( 'NONE',  ( 5.420926794907370727, 15.73778643695066393, 8.083040450566207014 ) ) ;
#7415 = CARTESIAN_POINT ( 'NONE',  ( -17.46249999999999858, 0.000000000000000000, 0.000000000000000000 ) ) ;
#7416 = VECTOR ( 'NONE', #10244, 1000.000000000000227 ) ;
#7417 = CIRCLE ( 'NONE', #10234, 1.984374999999999112 ) ;
#7418 = CARTESIAN_POINT ( 'NONE',  ( 5.593038387450195437, 14.77714803192029613, -1.122504005036815800 ) ) ;
#7419 = CYLINDRICAL_SURFACE ( 'NONE', #3302, 1.190625000000001155 ) ;
#7420 = VECTOR ( 'NONE', #18794, 1000.000000000000000 ) ;
#7421 = CARTESIAN_POINT ( 'NONE',  ( 11.07182980542974171, 10.97943152176106274, 4.054213205698371070 ) ) ;
#7422 = DIRECTION ( 'NONE',  ( 0.000000000000000000, -1.000000000000000000, -0.000000000000000000 ) ) ;
#7423 = CARTESIAN_POINT ( 'NONE',  ( 1.569416217892126708, 17.33683664400565050, 9.619349279799264352 ) ) ;
#7424 = CARTESIAN_POINT ( 'NONE',  ( 1.249608508386810257, 18.94596205324141280, 8.865697184473329884 ) ) ;
#7425 = CARTESIAN_POINT ( 'NONE',  ( 44.28293121686854761, 34.52875999999999834, -31.08068102505560759 ) ) ;
#7426 = CIRCLE ( 'NONE', #14504, 0.7950200000000003930 ) ;
#7427 = CARTESIAN_POINT ( 'NONE',  ( 7.037679341590383331, 18.17949408554134649, 7.363593253874445743 ) ) ;
#7428 = DIRECTION ( 'NONE',  ( -0.000000000000000000, -1.000000000000000000, 0.000000000000000000 ) ) ;
#7429 = DIRECTION ( 'NONE',  ( -0.08192867786951699149, 0.000000000000000000, -0.9966381950048638361 ) ) ;
#7430 = CARTESIAN_POINT ( 'NONE',  ( 15.78242036309661067, 2.283158471184189242, -15.52125926898847652 ) ) ;
#7431 = DIRECTION ( 'NONE',  ( -0.000000000000000000, -1.000000000000000000, 0.000000000000000000 ) ) ;
#7432 = EDGE_CURVE ( 'NONE', #218, #19957, #14171, .T. ) ;
#7433 = CARTESIAN_POINT ( 'NONE',  ( 11.38595208427108929, 13.73655500858925116, 6.976298811495518670 ) ) ;
#7434 = ORIENTED_EDGE ( 'NONE', *, *, #11131, .F. ) ;
#7435 = DIRECTION ( 'NONE',  ( 0.000000000000000000, 1.000000000000000000, 0.000000000000000000 ) ) ;
#7436 = CARTESIAN_POINT ( 'NONE',  ( 11.34624642647743720, 12.79290754381931627, -2.192977170836705181 ) ) ;
#7437 = AXIS2_PLACEMENT_3D ( 'NONE', #19295, #10796, #13606 ) ;
#7438 = CARTESIAN_POINT ( 'NONE',  ( 5.454630584850207242, 17.08472327719105266, -2.114810173200567966 ) ) ;
#7439 = CARTESIAN_POINT ( 'NONE',  ( -53.00154558624916490, -5.714999999999999858, -22.85927301266823264 ) ) ;
#7440 = CARTESIAN_POINT ( 'NONE',  ( 3.096978994538255314, 17.95937840445101230, 8.244996092440942448 ) ) ;
#7441 = AXIS2_PLACEMENT_3D ( 'NONE', #10348, #6917, #3495 ) ;
#7442 = VERTEX_POINT ( 'NONE', #7586 ) ;
#7443 = CARTESIAN_POINT ( 'NONE',  ( 21.25660046192028929, -1.983739999999999393, -13.18703856829094079 ) ) ;
#7444 = CARTESIAN_POINT ( 'NONE',  ( 9.275488759993784527, -7.547927499999999235, -20.77642327197297689 ) ) ;
#7445 = AXIS2_PLACEMENT_3D ( 'NONE', #2810, #6454, #16315 ) ;
#7446 = ORIENTED_EDGE ( 'NONE', *, *, #9890, .F. ) ;
#7447 = CARTESIAN_POINT ( 'NONE',  ( 7.653781805100536850, 13.15088303497838140, -1.081001487685353313 ) ) ;
#7448 =( GEOMETRIC_REPRESENTATION_CONTEXT ( 3 ) GLOBAL_UNCERTAINTY_ASSIGNED_CONTEXT ( ( #8560 ) ) GLOBAL_UNIT_ASSIGNED_CONTEXT ( ( #19486, #17735, #1022 ) ) REPRESENTATION_CONTEXT ( 'NONE', 'WORKASPACE' ) );
#7449 = CARTESIAN_POINT ( 'NONE',  ( 12.83050491244006786, 11.94611577877984132, 4.206736490311723031 ) ) ;
#7450 = DIRECTION ( 'NONE',  ( 0.000000000000000000, 1.000000000000000000, 0.000000000000000000 ) ) ;
#7451 = CARTESIAN_POINT ( 'NONE',  ( 10.88501636984964804, 16.27139374001615835, -4.462695918007991480 ) ) ;
#7452 = AXIS2_PLACEMENT_3D ( 'NONE', #3049, #21166, #11335 ) ;
#7453 = AXIS2_PLACEMENT_3D ( 'NONE', #3828, #7261, #175 ) ;
#7454 = CARTESIAN_POINT ( 'NONE',  ( 46.03750000000000142, 30.56064500000000095, -10.31874999999999964 ) ) ;
#7455 = CARTESIAN_POINT ( 'NONE',  ( 4.415627886922138146, 20.84303989866938878, 6.171506294094559308 ) ) ;
#7456 = CARTESIAN_POINT ( 'NONE',  ( 13.16124604336415338, 0.02081130280650461684, -16.33707070753825263 ) ) ;
#7457 = PRODUCT_DEFINITION_CONTEXT ( 'detailed design', #13024, 'design' ) ;
#7458 = PLANE ( 'NONE',  #19773 ) ;
#7459 = EDGE_CURVE ( 'NONE', #18381, #18451, #16966, .T. ) ;
#7460 = ORIENTED_EDGE ( 'NONE', *, *, #11667, .T. ) ;
#7461 = EDGE_CURVE ( 'NONE', #1622, #21739, #3639, .T. ) ;
#7462 = CARTESIAN_POINT ( 'NONE',  ( 10.32898373000674219, 10.45400687491624225, 2.198347703374553763 ) ) ;
#7463 = COLOUR_RGB ( '', 0.09019608, 0.27058824, 0.51372549) ;
#7464 = DIRECTION ( 'NONE',  ( 0.000000000000000000, -1.000000000000000000, -0.000000000000000000 ) ) ;
#7465 = ORIENTED_EDGE ( 'NONE', *, *, #5742, .F. ) ;
#7466 = CARTESIAN_POINT ( 'NONE',  ( 9.567093807291675134, 12.51404170299046648, -1.089912194315524330 ) ) ;
#7467 = CARTESIAN_POINT ( 'NONE',  ( 9.335363283976800375, 34.52875999999999834, -14.20581391854862474 ) ) ;
#7468 = CARTESIAN_POINT ( 'NONE',  ( 0.6844633117439506975, 19.47873662827283425, 7.356147931787495153 ) ) ;
#7470 = CARTESIAN_POINT ( 'NONE',  ( 12.76235139282079167, 21.25996874134203907, -20.69948241803004407 ) ) ;
#7469 = CARTESIAN_POINT ( 'NONE',  ( -1.273098367859926805, 20.20483442592724188, 3.536004553022368935 ) ) ;
#7471 = ORIENTED_EDGE ( 'NONE', *, *, #21036, .T. ) ;
#7472 = DIRECTION ( 'NONE',  ( 0.000000000000000000, 1.000000000000000000, 0.000000000000000000 ) ) ;
#7473 = VECTOR ( 'NONE', #1239, 1000.000000000000114 ) ;
#7474 = PLANE ( 'NONE',  #3476 ) ;
#7475 = AXIS2_PLACEMENT_3D ( 'NONE', #13305, #18254, #11622 ) ;
#7476 = VERTEX_POINT ( 'NONE', #4270 ) ;
#7477 = CARTESIAN_POINT ( 'NONE',  ( 19.50032822304632063, 0.3607342948534012494, -14.94848289734256852 ) ) ;
#7478 = CARTESIAN_POINT ( 'NONE',  ( 0.06129756055965347034, 14.31084331889941730, 1.337318312763465800 ) ) ;
#7479 = VECTOR ( 'NONE', #8832, 1000.000000000000114 ) ;
#7480 = CARTESIAN_POINT ( 'NONE',  ( 16.98959876662204849, 1.202893068749029126, -15.29982850647945369 ) ) ;
#7481 = ORIENTED_EDGE ( 'NONE', *, *, #19951, .F. ) ;
#7482 = DIRECTION ( 'NONE',  ( -0.3542738219355896501, 0.000000000000000000, -0.9351417320872542627 ) ) ;
#7483 = EDGE_CURVE ( 'NONE', #10833, #20627, #9195, .T. ) ;
#7484 = LINE ( 'NONE', #17657, #11737 ) ;
#7485 = DIRECTION ( 'NONE',  ( 0.2868778675745004558, 0.000000000000000000, 0.9579671649362035968 ) ) ;
#7486 = CARTESIAN_POINT ( 'NONE',  ( 39.62791084302666178, 0.000000000000000000, -24.65774797299118859 ) ) ;
#7487 =( GEOMETRIC_REPRESENTATION_CONTEXT ( 3 ) GLOBAL_UNCERTAINTY_ASSIGNED_CONTEXT ( ( #3929 ) ) GLOBAL_UNIT_ASSIGNED_CONTEXT ( ( #5164, #193, #5264 ) ) REPRESENTATION_CONTEXT ( 'NONE', 'WORKASPACE' ) );
#7488 = VECTOR ( 'NONE', #2438, 1000.000000000000114 ) ;
#7489 = VERTEX_POINT ( 'NONE', #12038 ) ;
#7490 = EDGE_CURVE ( 'NONE', #4077, #5219, #13817, .T. ) ;
#7491 = LINE ( 'NONE', #20849, #481 ) ;
#7493 = DIRECTION ( 'NONE',  ( -0.000000000000000000, -1.000000000000000000, 0.000000000000000000 ) ) ;
#7492 = DIRECTION ( 'NONE',  ( 0.05085730733808393328, 0.000000000000000000, -0.9987059298363656357 ) ) ;
#7494 = VERTEX_POINT ( 'NONE', #12462 ) ;
#7495 = VERTEX_POINT ( 'NONE', #19186 ) ;
#7497 = PLANE ( 'NONE',  #733 ) ;
#7496 = CARTESIAN_POINT ( 'NONE',  ( 5.499327144225777175, 17.51037618698124376, 8.771713425651105567 ) ) ;
#7498 = ORIENTED_EDGE ( 'NONE', *, *, #19356, .T. ) ;
#7499 = CARTESIAN_POINT ( 'NONE',  ( 5.591725253800921891, 15.70436773459850421, 8.761559460545525369 ) ) ;
#7500 = ADVANCED_FACE ( 'NONE', ( #17009 ), #725, .T. ) ;
#7501 = ORIENTED_EDGE ( 'NONE', *, *, #13815, .F. ) ;
#7502 = ORIENTED_EDGE ( 'NONE', *, *, #6976, .T. ) ;
#7503 = VECTOR ( 'NONE', #20972, 1000.000000000000000 ) ;
#7504 = VERTEX_POINT ( 'NONE', #1969 ) ;
#7505 = CARTESIAN_POINT ( 'NONE',  ( 2.803679754229469800, 12.09773929403007031, 4.926693614680812239 ) ) ;
#7506 = EDGE_CURVE ( 'NONE', #7172, #9498, #381, .T. ) ;
#7507 = EDGE_CURVE ( 'NONE', #1876, #3944, #2519, .T. ) ;
#7508 = CIRCLE ( 'NONE', #20920, 0.7950200000000000600 ) ;
#7509 = ADVANCED_FACE ( 'NONE', ( #20307 ), #14346, .F. ) ;
#7510 =( GEOMETRIC_REPRESENTATION_CONTEXT ( 3 ) GLOBAL_UNCERTAINTY_ASSIGNED_CONTEXT ( ( #5688 ) ) GLOBAL_UNIT_ASSIGNED_CONTEXT ( ( #16367, #7836, #19761 ) ) REPRESENTATION_CONTEXT ( 'NONE', 'WORKASPACE' ) );
#7511 = CARTESIAN_POINT ( 'NONE',  ( 65.64431122251959039, 30.56064500000000095, -11.29787305743958115 ) ) ;
#7512 = DIRECTION ( 'NONE',  ( 0.000000000000000000, -1.000000000000000000, -0.000000000000000000 ) ) ;
#7513 = CARTESIAN_POINT ( 'NONE',  ( 1.337733264118907694, 23.41816499999999834, 8.634866101730979793 ) ) ;
#7514 = DIRECTION ( 'NONE',  ( 0.000000000000000000, 1.000000000000000000, 0.000000000000000000 ) ) ;
#7515 = CARTESIAN_POINT ( 'NONE',  ( 2.433075215497880972, 20.76646021035401901, 6.507622753141381722 ) ) ;
#7516 = ORIENTED_EDGE ( 'NONE', *, *, #5352, .T. ) ;
#7517 = CARTESIAN_POINT ( 'NONE',  ( 1.533183450453754704, 12.01664638779708127, 6.289946621455513309 ) ) ;
#7518 = CARTESIAN_POINT ( 'NONE',  ( 10.72409186464205355, -4.809670885807086016, -15.96177715662992824 ) ) ;
#7519 = CARTESIAN_POINT ( 'NONE',  ( 13.35334803189539521, 22.16103170555246393, 1.961556584310249596 ) ) ;
#7520 = DIRECTION ( 'NONE',  ( 0.000000000000000000, 1.000000000000000000, 0.000000000000000000 ) ) ;
#7521 = DIRECTION ( 'NONE',  ( 0.2490110332224850509, 0.000000000000000000, -0.9685006480810792739 ) ) ;
#7522 = AXIS2_PLACEMENT_3D ( 'NONE', #11379, #16148, #9598 ) ;
#7523 = ORIENTED_EDGE ( 'NONE', *, *, #17168, .T. ) ;
#7524 = ORIENTED_EDGE ( 'NONE', *, *, #4449, .T. ) ;
#7525 = CARTESIAN_POINT ( 'NONE',  ( 12.88673784487023255, 14.76516699303951619, 6.813854300165841593 ) ) ;
#7526 = DIRECTION ( 'NONE',  ( 0.2490110332224850509, 0.000000000000000000, -0.9685006480810792739 ) ) ;
#7527 = CARTESIAN_POINT ( 'NONE',  ( 12.95722427598218118, 11.51533396550468247, 4.774218139127305527 ) ) ;
#7528 = ORIENTED_EDGE ( 'NONE', *, *, #15943, .F. ) ;
#7529 = ORIENTED_EDGE ( 'NONE', *, *, #11602, .T. ) ;
#7530 = CARTESIAN_POINT ( 'NONE',  ( 46.03750000000000142, 0.000000000000000000, -10.31874999999999964 ) ) ;
#7531 = CARTESIAN_POINT ( 'NONE',  ( 7.882649901787743829, 20.03851403430508782, -1.570039674128517859 ) ) ;
#7532 = CARTESIAN_POINT ( 'NONE',  ( 7.377632332484820310, 14.94885212140055408, 7.515399275738874785 ) ) ;
#7533 = CARTESIAN_POINT ( 'NONE',  ( 65.90927232300019512, 30.56064500000000095, -13.30734117861468135 ) ) ;
#7534 = CARTESIAN_POINT ( 'NONE',  ( 6.517250350420195737, 20.15272355558845874, 0.5064415424127612919 ) ) ;
#7535 = CARTESIAN_POINT ( 'NONE',  ( 2.152814512047750650, 20.23805962733014852, 5.716278487167510747 ) ) ;
#7536 = CARTESIAN_POINT ( 'NONE',  ( 39.00487391864218267, 37.69864044684034354, -3.894748490052650780 ) ) ;
#7537 = EDGE_CURVE ( 'NONE', #2498, #18746, #9210, .T. ) ;
#7538 = AXIS2_PLACEMENT_3D ( 'NONE', #2177, #8919, #298 ) ;
#7539 = EDGE_CURVE ( 'NONE', #6164, #17225, #8156, .T. ) ;
#7540 = CARTESIAN_POINT ( 'NONE',  ( 8.881999483277855489, 20.20358612698620249, 6.571188270847311941 ) ) ;
#7541 = DIRECTION ( 'NONE',  ( 0.9685006480810792739, 0.000000000000000000, 0.2490110332224850509 ) ) ;
#7542 = CARTESIAN_POINT ( 'NONE',  ( 3.463643476966617119, 15.44861990895924819, -1.447185448056517831 ) ) ;
#7543 = LINE ( 'NONE', #578, #6114 ) ;
#7544 = CIRCLE ( 'NONE', #20224, 0.7950199999999993938 ) ;
#7545 = LINE ( 'NONE', #21123, #16369 ) ;
#7546 = CARTESIAN_POINT ( 'NONE',  ( 1.459627900731261141, 14.30699635049795226, 8.431327355238760646 ) ) ;
#7547 = CARTESIAN_POINT ( 'NONE',  ( 52.96420052373725440, 32.54502000000000095, 7.017842122255405712 ) ) ;
#7548 = CYLINDRICAL_SURFACE ( 'NONE', #755, 9.524999999999996803 ) ;
#7549 = CARTESIAN_POINT ( 'NONE',  ( 11.50671703646502131, -0.1979220242447447820, -16.81508318434922344 ) ) ;
#7550 = ORIENTED_EDGE ( 'NONE', *, *, #6110, .F. ) ;
#7551 = CARTESIAN_POINT ( 'NONE',  ( 3.360635606688116894, 34.52875999999999834, -20.45316710734507026 ) ) ;
#7552 = CARTESIAN_POINT ( 'NONE',  ( 10.94369443579043200, 11.39479583509590199, 4.876173924909795510 ) ) ;
#7553 = ORIENTED_EDGE ( 'NONE', *, *, #18555, .F. ) ;
#7554 = CIRCLE ( 'NONE', #20243, 0.7950200000000005041 ) ;
#7555 = LINE ( 'NONE', #5549, #11006 ) ;
#7556 = CARTESIAN_POINT ( 'NONE',  ( 5.572600844917717566, 12.66182956979191587, -0.7461097123436445377 ) ) ;
#7557 = CARTESIAN_POINT ( 'NONE',  ( 29.98909767165928386, 2.019535839764540430, -5.214162619065493054 ) ) ;
#7558 = EDGE_LOOP ( 'NONE', ( #14156, #4502, #6471 ) ) ;
#7559 = CARTESIAN_POINT ( 'NONE',  ( 0.1129728326432310886, 20.32260066561571676, 5.061726021590057023 ) ) ;
#7560 = CARTESIAN_POINT ( 'NONE',  ( 57.23009918853844624, 0.000000000000000000, -20.42665903041912401 ) ) ;
#7561 = VECTOR ( 'NONE', #20679, 1000.000000000000114 ) ;
#7562 = ADVANCED_FACE ( 'NONE', ( #15269 ), #15381, .T. ) ;
#7563 = CARTESIAN_POINT ( 'NONE',  ( 11.44847493648600611, -6.403249497899589748, -17.02820558865678535 ) ) ;
#7564 = EDGE_LOOP ( 'NONE', ( #14812, #18530, #3818, #4353 ) ) ;
#7565 = CARTESIAN_POINT ( 'NONE',  ( 12.85337560073962493, 21.48306739246610420, 0.4997394630849344432 ) ) ;
#7566 = CARTESIAN_POINT ( 'NONE',  ( 4.614827001460207079, 19.61000027071614227, 6.590015868446513991 ) ) ;
#7567 = VECTOR ( 'NONE', #6173, 1000.000000000000000 ) ;
#7568 = CARTESIAN_POINT ( 'NONE',  ( 11.26774977721790449, 15.74974973885002250, 6.878961729585737039 ) ) ;
#7569 = CARTESIAN_POINT ( 'NONE',  ( 13.99789750971088331, 21.64220180175570363, 3.696402113709151394 ) ) ;
#7570 = CARTESIAN_POINT ( 'NONE',  ( 53.35709526732357233, -7.529133977686723433, -16.41569776986803930 ) ) ;
#7571 = CARTESIAN_POINT ( 'NONE',  ( 3.861847520083515839, 21.32356625081728296, 4.680827701663748286 ) ) ;
#7572 = DIRECTION ( 'NONE',  ( -0.4128958666089267981, 0.5884034904305870395, 0.6951966166390379787 ) ) ;
#7573 = VERTEX_POINT ( 'NONE', #19943 ) ;
#7574 = CARTESIAN_POINT ( 'NONE',  ( 14.25008779104191703, 21.25436666907090455, 4.245038886465763106 ) ) ;
#7575 = CIRCLE ( 'NONE', #9680, 0.5079999999999996740 ) ;
#7576 = DIRECTION ( 'NONE',  ( 0.000000000000000000, 1.000000000000000000, 0.000000000000000000 ) ) ;
#7577 = ORIENTED_EDGE ( 'NONE', *, *, #15750, .F. ) ;
#7578 = CARTESIAN_POINT ( 'NONE',  ( 11.88155870319460128, 20.88804905822066971, 3.524732118264728875 ) ) ;
#7579 = DIRECTION ( 'NONE',  ( -0.9173788132826627972, 0.000000000000000000, 0.3980152169705239440 ) ) ;
#7580 = CARTESIAN_POINT ( 'NONE',  ( 0.2225936923515433874, 20.08366710440301262, 6.197720518317566096 ) ) ;
#7582 = DIRECTION ( 'NONE',  ( -0.08420877549337300871, 0.000000000000000000, -0.9964481331860212121 ) ) ;
#7581 = CARTESIAN_POINT ( 'NONE',  ( 5.703860639285195155, 11.35334887747070276, 1.266263560432865143 ) ) ;
#7583 = EDGE_LOOP ( 'NONE', ( #2688, #17869 ) ) ;
#7584 =( NAMED_UNIT ( * ) SI_UNIT ( $, .STERADIAN. ) SOLID_ANGLE_UNIT ( ) );
#7585 = AXIS2_PLACEMENT_3D ( 'NONE', #20538, #3533, #8613 ) ;
#7586 = CARTESIAN_POINT ( 'NONE',  ( -7.949728765565600597, 33.32892749999999893, -34.47798802950714503 ) ) ;
#7587 = CARTESIAN_POINT ( 'NONE',  ( 38.96848998618624904, -5.166360000000000063, -3.934807454472129429 ) ) ;
#7588 = VERTEX_POINT ( 'NONE', #12908 ) ;
#7589 = CARTESIAN_POINT ( 'NONE',  ( 12.11879977990919421, 13.08893749999999834, 0.1373704394269426865 ) ) ;
#7590 = EDGE_CURVE ( 'NONE', #19114, #9035, #9563, .T. ) ;
#7591 = CARTESIAN_POINT ( 'NONE',  ( 11.61881240165799944, -3.657972840441829465, -15.65996692772725041 ) ) ;
#7592 = ORIENTED_EDGE ( 'NONE', *, *, #7224, .T. ) ;
#7593 = CARTESIAN_POINT ( 'NONE',  ( -3.037751992662818257, 28.56769750000000130, -30.02724401157551526 ) ) ;
#7594 = CARTESIAN_POINT ( 'NONE',  ( 1.881684930349333928, 15.09886263991730537, 0.2569686833294808626 ) ) ;
#7595 = CIRCLE ( 'NONE', #18886, 1.984374999999999112 ) ;
#7596 = DIRECTION ( 'NONE',  ( 0.000000000000000000, -1.000000000000000000, 0.000000000000000000 ) ) ;
#7597 = EDGE_LOOP ( 'NONE', ( #18186, #13151, #16349, #6817 ) ) ;
#7598 = CARTESIAN_POINT ( 'NONE',  ( 49.13030338002142372, 109.3223030719999969, -2.154981381712871791 ) ) ;
#7599 = CARTESIAN_POINT ( 'NONE',  ( 39.11241740126524746, -7.547728945059590799, -4.078053966296677935 ) ) ;
#7600 = EDGE_LOOP ( 'NONE', ( #20959, #11676, #3016, #6406, #3970 ) ) ;
#7601 = ORIENTED_EDGE ( 'NONE', *, *, #2239, .T. ) ;
#7602 = DIRECTION ( 'NONE',  ( 0.000000000000000000, -1.000000000000000000, 0.000000000000000000 ) ) ;
#7604 = DIRECTION ( 'NONE',  ( 0.08420877549337300871, 0.000000000000000000, 0.9964481331860212121 ) ) ;
#7603 = CARTESIAN_POINT ( 'NONE',  ( 1.745695617745230299, 15.58894874012881182, 9.651474225904069115 ) ) ;
#7605 = EDGE_LOOP ( 'NONE', ( #11132, #20151, #9309, #19548 ) ) ;
#7606 = CARTESIAN_POINT ( 'NONE',  ( 3.835900461743189549, 12.20702721357838172, 0.5463839515351021081 ) ) ;
#7607 = ADVANCED_FACE ( 'NONE', ( #13120 ), #19718, .F. ) ;
#7608 = ORIENTED_EDGE ( 'NONE', *, *, #5863, .T. ) ;
#7609 = ORIENTED_EDGE ( 'NONE', *, *, #8322, .T. ) ;
#7610 = AXIS2_PLACEMENT_3D ( 'NONE', #18273, #13215, #13105 ) ;
#7611 = EDGE_CURVE ( 'NONE', #3414, #3770, #14890, .T. ) ;
#7612 = ORIENTED_EDGE ( 'NONE', *, *, #13734, .T. ) ;
#7613 = EDGE_CURVE ( 'NONE', #1856, #15382, #11339, .T. ) ;
#7614 = EDGE_CURVE ( 'NONE', #10018, #21869, #1048, .T. ) ;
#7615 = DIRECTION ( 'NONE',  ( -0.08420877549337300871, 0.000000000000000000, -0.9964481331860212121 ) ) ;
#7616 = CARTESIAN_POINT ( 'NONE',  ( 66.79943102505561114, 34.52875999999999834, -12.07331878313145168 ) ) ;
#7617 = DIRECTION ( 'NONE',  ( -0.6744690509234928522, -0.7360996206939028896, 0.05699866455150636585 ) ) ;
#7618 = CARTESIAN_POINT ( 'NONE',  ( 17.79723720954694954, -1.983739999999999393, -14.07647485258271303 ) ) ;
#7619 = CARTESIAN_POINT ( 'NONE',  ( 2.547717337248343039, 11.27265232115933102, 3.789480751304223460 ) ) ;
#7620 = EDGE_LOOP ( 'NONE', ( #2836, #11792, #1234, #5025 ) ) ;
#7621 = DIRECTION ( 'NONE',  ( 0.8609107660235849613, 0.000000000000000000, -0.5087559856598092844 ) ) ;
#7622 = CARTESIAN_POINT ( 'NONE',  ( 9.256853431388732290, -1.983739999999999393, -17.09316853730597074 ) ) ;
#7623 = FILL_AREA_STYLE ('',( #11052 ) ) ;
#7624 = VERTEX_POINT ( 'NONE', #6347 ) ;
#7625 = ORIENTED_EDGE ( 'NONE', *, *, #16956, .F. ) ;
#7626 = CARTESIAN_POINT ( 'NONE',  ( 10.44189738732276140, 19.34515354661070319, 6.540544623818083103 ) ) ;
#7628 = DIRECTION ( 'NONE',  ( -0.8583349619704301325, 0.000000000000000000, 0.5130897514657842828 ) ) ;
#7627 = LINE ( 'NONE', #12843, #950 ) ;
#7629 = CARTESIAN_POINT ( 'NONE',  ( 11.58355748138406938, 10.94906613365873049, -0.9808765445798767191 ) ) ;
#7630 = VERTEX_POINT ( 'NONE', #21608 ) ;
#7631 = EDGE_CURVE ( 'NONE', #15924, #20164, #16537, .T. ) ;
#7632 = ORIENTED_EDGE ( 'NONE', *, *, #20484, .T. ) ;
#7633 = DIRECTION ( 'NONE',  ( 0.2868778675745010664, 0.000000000000000000, 0.9579671649362032637 ) ) ;
#7634 = PRODUCT_RELATED_PRODUCT_CATEGORY ( 'part', '', ( #9124 ) ) ;
#7635 = CARTESIAN_POINT ( 'NONE',  ( 7.521814107298904872, 12.14759314724596706, -1.039252882385111709 ) ) ;
#7636 = CARTESIAN_POINT ( 'NONE',  ( -2.028188046367890074, 9.129395000000000593, 0.3682158094503220069 ) ) ;
#7637 = DIRECTION ( 'NONE',  ( 0.08420877549337300871, 0.000000000000000000, 0.9964481331860212121 ) ) ;
#7638 = CARTESIAN_POINT ( 'NONE',  ( 8.458318833295095374, 19.91303329138582257, 5.610345679553954135 ) ) ;
#7639 = ADVANCED_FACE ( 'NONE', ( #11005, #9449 ), #14562, .F. ) ;
#7640 = EDGE_CURVE ( 'NONE', #21414, #9339, #16311, .T. ) ;
#7641 = CARTESIAN_POINT ( 'NONE',  ( -3.929154139288399961, 9.129395000000000593, 0.9374890779182719625 ) ) ;
#7642 = CARTESIAN_POINT ( 'NONE',  ( 7.001331565757744180, 11.28301579719734171, 5.025527442906016162 ) ) ;
#7643 = FACE_OUTER_BOUND ( 'NONE', #8763, .T. ) ;
#7644 = LINE ( 'NONE', #16386, #12704 ) ;
#7645 = CARTESIAN_POINT ( 'NONE',  ( 4.370808908492361589, 20.54241105020114233, 0.3984924473438536396 ) ) ;
#7646 = CARTESIAN_POINT ( 'NONE',  ( 1.685730993150120982, 15.98818651832521809, 9.604930218560687294 ) ) ;
#7647 = FACE_OUTER_BOUND ( 'NONE', #15764, .T. ) ;
#7648 = CARTESIAN_POINT ( 'NONE',  ( 3.435969853487951031, 14.96929529427155714, 8.323793337960825767 ) ) ;
#7649 = DIRECTION ( 'NONE',  ( 0.000000000000000000, -1.000000000000000000, 0.000000000000000000 ) ) ;
#7650 = CARTESIAN_POINT ( 'NONE',  ( 49.28028498622276032, 34.52875999999999834, -25.68670502218146368 ) ) ;
#7651 = CARTESIAN_POINT ( 'NONE',  ( 13.54613991325937583, 1.731347537946924309, -16.18443696118438524 ) ) ;
#7652 = ORIENTED_EDGE ( 'NONE', *, *, #11927, .T. ) ;
#7653 = CYLINDRICAL_SURFACE ( 'NONE', #13825, 1.190625000000000711 ) ;
#7654 = CARTESIAN_POINT ( 'NONE',  ( 11.39404450035965510, 13.83933078011801499, 7.025478403630279978 ) ) ;
#7655 = ORIENTED_EDGE ( 'NONE', *, *, #11833, .F. ) ;
#7656 = ADVANCED_FACE ( 'NONE', ( #7689 ), #13234, .T. ) ;
#7657 = LINE ( 'NONE', #19592, #7821 ) ;
#7658 = ADVANCED_FACE ( 'NONE', ( #14449 ), #11119, .F. ) ;
#7659 = CARTESIAN_POINT ( 'NONE',  ( 11.82169470351746732, 19.85945549919958353, -2.282691836462475088 ) ) ;
#7660 = EDGE_CURVE ( 'NONE', #14970, #14236, #12794, .T. ) ;
#7661 = CARTESIAN_POINT ( 'NONE',  ( 5.736873335961724329, 11.96313308795059172, 0.01662313235952948484 ) ) ;
#7662 = FACE_OUTER_BOUND ( 'NONE', #14267, .T. ) ;
#7663 = ORIENTED_EDGE ( 'NONE', *, *, #8093, .T. ) ;
#7664 = LINE ( 'NONE', #6215, #21222 ) ;
#7665 = CIRCLE ( 'NONE', #14389, 0.7950200000000003930 ) ;
#7666 = DIRECTION ( 'NONE',  ( 0.2868778675745011220, 0.000000000000000000, 0.9579671649362034858 ) ) ;
#7667 = VERTEX_POINT ( 'NONE', #14782 ) ;
#7668 = CARTESIAN_POINT ( 'NONE',  ( 5.835913855334317724, 15.55272378482423079, -1.593939421784943189 ) ) ;
#7669 = CARTESIAN_POINT ( 'NONE',  ( 5.336950776178195355, 16.31355649014509623, 8.043007501857138308 ) ) ;
#7670 = CARTESIAN_POINT ( 'NONE',  ( 8.958927231525365187, 12.18567386761292148, 5.087176938866648790 ) ) ;
#7671 = CARTESIAN_POINT ( 'NONE',  ( 2.105188602693566224, 13.07595850747188315, 0.3638253081235816588 ) ) ;
#7672 = CYLINDRICAL_SURFACE ( 'NONE', #13521, 0.7950199999999982836 ) ;
#7673 = FACE_OUTER_BOUND ( 'NONE', #21179, .T. ) ;
#7674 = CARTESIAN_POINT ( 'NONE',  ( 43.29176983217143260, 32.54502000000000095, 5.154088326438659884 ) ) ;
#7675 = CARTESIAN_POINT ( 'NONE',  ( 1.268730000000000135, 24.21318500000000284, 69.04070710741299877 ) ) ;
#7676 = CIRCLE ( 'NONE', #2740, 0.5079999999999996740 ) ;
#7677 = ORIENTED_EDGE ( 'NONE', *, *, #14838, .T. ) ;
#7678 = B_SPLINE_CURVE_WITH_KNOTS ( 'NONE', 3,
 ( #20188, #10038, #8365, #15138 ),
 .UNSPECIFIED., .F., .F.,
 ( 4, 4 ),
 ( -7.968845587668732479E-05, 0.0007517676470877217038 ),
 .UNSPECIFIED. ) ;
#7679 = CARTESIAN_POINT ( 'NONE',  ( 20.48971467568342675, -6.006590701077150207, -13.94752972188701534 ) ) ;
#7680 = CYLINDRICAL_SURFACE ( 'NONE', #3503, 3.174999999999997158 ) ;
#7681 = ORIENTED_EDGE ( 'NONE', *, *, #5768, .F. ) ;
#7682 = EDGE_CURVE ( 'NONE', #12681, #8349, #3228, .T. ) ;
#7683 = CARTESIAN_POINT ( 'NONE',  ( 10.59060266505083803, 20.91478602822554222, 0.04984095317570090555 ) ) ;
#7684 = LINE ( 'NONE', #21485, #17649 ) ;
#7685 = DIRECTION ( 'NONE',  ( -0.7776383362760926898, 0.000000000000000000, 0.6287118719681938916 ) ) ;
#7687 = DIRECTION ( 'NONE',  ( 0.9685006480810792739, 0.000000000000000000, 0.2490110332224850509 ) ) ;
#7686 = CARTESIAN_POINT ( 'NONE',  ( 4.178641076556762535, 20.20829226350481989, 6.748569037004350513 ) ) ;
#7688 = ORIENTED_EDGE ( 'NONE', *, *, #6976, .F. ) ;
#7689 = FACE_OUTER_BOUND ( 'NONE', #16105, .T. ) ;
#7690 = CARTESIAN_POINT ( 'NONE',  ( 39.79795571586765845, -6.669711430507633487, -3.121712638490365510 ) ) ;
#7691 = ORIENTED_EDGE ( 'NONE', *, *, #9143, .T. ) ;
#7692 = CARTESIAN_POINT ( 'NONE',  ( -4.157227781567939928, 9.924415000000001541, 0.1758860224507720060 ) ) ;
#7693 = AXIS2_PLACEMENT_3D ( 'NONE', #16492, #16711, #1438 ) ;
#7694 = CARTESIAN_POINT ( 'NONE',  ( 17.47713756659358353, -7.126243325886450819, -14.69286177225622225 ) ) ;
#7695 = VERTEX_POINT ( 'NONE', #1163 ) ;
#7696 = CARTESIAN_POINT ( 'NONE',  ( 8.170949848228001855, 11.48768387232824217, 1.861147236350632728 ) ) ;
#7697 = CARTESIAN_POINT ( 'NONE',  ( 2.188904998575694538, 18.20681673484682861, 0.4591847818817980653 ) ) ;
#7698 = CARTESIAN_POINT ( 'NONE',  ( 20.37526559019908134, -1.303711368126346581, -14.71844211684304504 ) ) ;
#7699 = FACE_BOUND ( 'NONE', #7620, .T. ) ;
#7700 = EDGE_LOOP ( 'NONE', ( #1840, #14772, #12923, #17093 ) ) ;
#7701 = DIRECTION ( 'NONE',  ( -0.4987171968201928873, 0.000000000000000000, 0.8667647648559606566 ) ) ;
#7703 = CARTESIAN_POINT ( 'NONE',  ( -29.36874999999999858, 1.983739999999999837, 10.71562499999999929 ) ) ;
#7702 = FACE_OUTER_BOUND ( 'NONE', #1940, .T. ) ;
#7704 = ORIENTED_EDGE ( 'NONE', *, *, #4898, .T. ) ;
#7705 = VERTEX_POINT ( 'NONE', #2716 ) ;
#7706 = EDGE_CURVE ( 'NONE', #9189, #3005, #2823, .T. ) ;
#7707 = AXIS2_PLACEMENT_3D ( 'NONE', #3723, #3612, #5369 ) ;
#7708 = CARTESIAN_POINT ( 'NONE',  ( 21.26534678900696562, -2.646493446368754388, -13.76446654770388811 ) ) ;
#7710 = DIRECTION ( 'NONE',  ( 0.000000000000000000, 1.000000000000000000, 0.000000000000000000 ) ) ;
#7709 = CARTESIAN_POINT ( 'NONE',  ( 6.742783883146333146, 10.91793053508332001, 4.244188499288108929 ) ) ;
#7711 = ORIENTED_EDGE ( 'NONE', *, *, #11479, .T. ) ;
#7712 = CARTESIAN_POINT ( 'NONE',  ( 3.939194837300639573, 19.06718353162318991, -0.7130797351348172608 ) ) ;
#7713 = ORIENTED_EDGE ( 'NONE', *, *, #16577, .F. ) ;
#7714 = VERTEX_POINT ( 'NONE', #21281 ) ;
#7715 = CARTESIAN_POINT ( 'NONE',  ( 52.27714366836601556, -6.669713112672388533, -17.51569705283379363 ) ) ;
#7716 = ORIENTED_EDGE ( 'NONE', *, *, #10174, .T. ) ;
#7717 = CARTESIAN_POINT ( 'NONE',  ( 3.145532673433270698, 12.72872530801424240, 6.528795813461734099 ) ) ;
#7718 = CIRCLE ( 'NONE', #7363, 0.5953125000000004663 ) ;
#7719 = CARTESIAN_POINT ( 'NONE',  ( -19.26602273594821924, 38.49687500000000284, -73.22163862549463431 ) ) ;
#7720 = DIRECTION ( 'NONE',  ( 0.000000000000000000, 1.000000000000000000, 0.000000000000000000 ) ) ;
#7721 = DIRECTION ( 'NONE',  ( 0.000000000000000000, -1.000000000000000000, -0.000000000000000000 ) ) ;
#7722 = DIRECTION ( 'NONE',  ( 0.000000000000000000, 1.000000000000000000, 0.000000000000000000 ) ) ;
#7723 = CARTESIAN_POINT ( 'NONE',  ( 2.876035228143350331, 11.34340886899239109, 5.205579515552751779 ) ) ;
#7724 = ORIENTED_EDGE ( 'NONE', *, *, #18775, .T. ) ;
#7725 = DIRECTION ( 'NONE',  ( 0.9964481331860212121, 0.000000000000000000, -0.08420877549337300871 ) ) ;
#7726 = DIRECTION ( 'NONE',  ( 0.05085730733808139364, 0.000000000000000000, -0.9987059298363658577 ) ) ;
#7727 = DIRECTION ( 'NONE',  ( -0.9685006480810792739, 0.000000000000000000, -0.2490110332224846346 ) ) ;
#7728 = CARTESIAN_POINT ( 'NONE',  ( 53.69636427252483202, 38.88803500000000213, -18.48840734645144224 ) ) ;
#7729 = VECTOR ( 'NONE', #301, 1000.000000000000000 ) ;
#7730 = ORIENTED_EDGE ( 'NONE', *, *, #10267, .T. ) ;
#7731 = ORIENTED_EDGE ( 'NONE', *, *, #4721, .T. ) ;
#7732 = EDGE_CURVE ( 'NONE', #6199, #21155, #9559, .T. ) ;
#7733 = CARTESIAN_POINT ( 'NONE',  ( 7.331740208057938801, 18.10524492707348898, -1.926982220310529570 ) ) ;
#7734 = EDGE_CURVE ( 'NONE', #2217, #1202, #19799, .T. ) ;
#7736 = CYLINDRICAL_SURFACE ( 'NONE', #2531, 0.5953125000000005773 ) ;
#7735 = LINE ( 'NONE', #9606, #2363 ) ;
#7737 = CARTESIAN_POINT ( 'NONE',  ( 10.94579177605037579, 14.27302213158844602, -3.976339498359578339 ) ) ;
#7738 = ORIENTED_EDGE ( 'NONE', *, *, #8968, .T. ) ;
#7739 = EDGE_LOOP ( 'NONE', ( #16969, #15017, #17119, #12216, #9476, #6518, #4147, #17345, #765, #15243, #1162, #11983, #16920, #3994, #20719, #20363, #15810, #1067, #9963, #197, #7952, #15890, #3036, #12433, #5519, #18852, #17783 ) ) ;
#7740 = CARTESIAN_POINT ( 'NONE',  ( -2.607150795738780058, 0.000000000000000000, 8.731885000000000119 ) ) ;
#7741 = VECTOR ( 'NONE', #8594, 1000.000000000000227 ) ;
#7742 = CARTESIAN_POINT ( 'NONE',  ( 7.698216182924317863, 11.55586773472163209, -0.2515938179596974300 ) ) ;
#7743 = CARTESIAN_POINT ( 'NONE',  ( 6.966837752621037438, 20.72930966971181377, 1.679252894246652028 ) ) ;
#7744 = AXIS2_PLACEMENT_3D ( 'NONE', #16986, #1839, #8580 ) ;
#7745 = DIRECTION ( 'NONE',  ( 0.000000000000000000, 1.000000000000000000, 0.000000000000000000 ) ) ;
#7746 = VECTOR ( 'NONE', #20115, 1000.000000000000000 ) ;
#7747 = CARTESIAN_POINT ( 'NONE',  ( 11.26444812368913873, 12.02016517962410269, 5.847082729819134350 ) ) ;
#7748 = EDGE_CURVE ( 'NONE', #3547, #3091, #13123, .T. ) ;
#7749 = FACE_BOUND ( 'NONE', #11573, .T. ) ;
#7750 = FACE_OUTER_BOUND ( 'NONE', #12553, .T. ) ;
#7751 = CARTESIAN_POINT ( 'NONE',  ( 5.965713978883512070, 11.27437957348430153, 1.153757586229308574 ) ) ;
#7752 = CARTESIAN_POINT ( 'NONE',  ( 1.704162562805419778, 15.26834743306047670, 9.500263804380585597 ) ) ;
#7753 = DIRECTION ( 'NONE',  ( 0.000000000000000000, -1.000000000000000000, 0.000000000000000000 ) ) ;
#7754 = CARTESIAN_POINT ( 'NONE',  ( 1.566762436808580850, 14.30904236277701003, 8.395310680802657188 ) ) ;
#7755 = CARTESIAN_POINT ( 'NONE',  ( 1.883521391995739203, 23.69003045368055282, 10.71562500000000107 ) ) ;
#7756 = FACE_BOUND ( 'NONE', #4257, .T. ) ;
#7757 = CARTESIAN_POINT ( 'NONE',  ( 18.96717912055868638, -7.261914202138213703, -14.21728248528548200 ) ) ;
#7758 = EDGE_LOOP ( 'NONE', ( #5277, #13457, #21545, #21165, #10103, #20040 ) ) ;
#7759 = PLANE ( 'NONE',  #8873 ) ;
#7760 = EDGE_CURVE ( 'NONE', #7279, #13567, #3284, .T. ) ;
#7761 = CARTESIAN_POINT ( 'NONE',  ( 11.44084217265526071, 14.79698256115047350, 7.380351338282362228 ) ) ;
#7762 = ORIENTED_EDGE ( 'NONE', *, *, #7506, .T. ) ;
#7763 = CARTESIAN_POINT ( 'NONE',  ( 25.61392306623480053, 1.050555293943630009, 10.48268080777146061 ) ) ;
#7764 = CARTESIAN_POINT ( 'NONE',  ( 12.19555853789111310, 20.67832640328533600, -1.317058961510981785 ) ) ;
#7765 = CARTESIAN_POINT ( 'NONE',  ( 5.520456159175803457, 17.64984982689927762, -2.012547465800341495 ) ) ;
#7766 = CARTESIAN_POINT ( 'NONE',  ( 8.011380105705496746, 34.12394749999999988, -19.05252355006962617 ) ) ;
#7767 = CARTESIAN_POINT ( 'NONE',  ( 0.1533679602575867273, 17.19689764357661943, 0.7834172150352086694 ) ) ;
#7768 = VERTEX_POINT ( 'NONE', #16452 ) ;
#7769 = EDGE_CURVE ( 'NONE', #20984, #2328, #15958, .T. ) ;
#7770 = AXIS2_PLACEMENT_3D ( 'NONE', #21488, #13012, #17971 ) ;
#7771 = CARTESIAN_POINT ( 'NONE',  ( 21.45456921355305724, -14.84248999999999974, -13.95701595352872815 ) ) ;
#7772 = CARTESIAN_POINT ( 'NONE',  ( 10.40081950133698818, 20.33297925226851888, -1.342766371799479330 ) ) ;
#7773 = ADVANCED_FACE ( 'NONE', ( #13251 ), #13137, .T. ) ;
#7774 = CIRCLE ( 'NONE', #20454, 30.16249999999998721 ) ;
#7775 = CARTESIAN_POINT ( 'NONE',  ( 23.00195419928544638, 3.565842500000000914, -15.19829965147284945 ) ) ;
#7776 = EDGE_CURVE ( 'NONE', #3833, #7070, #19850, .T. ) ;
#7777 = CARTESIAN_POINT ( 'NONE',  ( -15.27935546639805331, -5.951855000000001006, -26.04713531390440906 ) ) ;
#7778 = EDGE_CURVE ( 'NONE', #16850, #14366, #9685, .T. ) ;
#7779 = CARTESIAN_POINT ( 'NONE',  ( 32.52436584422698473, 32.54502000000000095, 1.884807767196291284 ) ) ;
#7780 = LINE ( 'NONE', #17326, #9719 ) ;
#7781 = CARTESIAN_POINT ( 'NONE',  ( 20.99038978835910640, -4.695846652395300858, -15.04226715606432663 ) ) ;
#7782 = DIRECTION ( 'NONE',  ( -0.5087559856598092844, 0.000000000000000000, -0.8609107660235849613 ) ) ;
#7783 = CIRCLE ( 'NONE', #7069, 0.7950200000000000600 ) ;
#7784 = ORIENTED_EDGE ( 'NONE', *, *, #7490, .F. ) ;
#7785 = DIRECTION ( 'NONE',  ( -0.2490110332224869660, -9.093548366658288884E-16, 0.9685006480810788299 ) ) ;
#7786 = VERTEX_POINT ( 'NONE', #16342 ) ;
#7787 = CARTESIAN_POINT ( 'NONE',  ( 12.16163452745204232, 20.48856804812561450, 4.265005074572522759 ) ) ;
#7788 = CARTESIAN_POINT ( 'NONE',  ( 1.477062725962008827, 15.58526859550301147, 8.784116692769741164 ) ) ;
#7789 = CARTESIAN_POINT ( 'NONE',  ( 20.32941413478750547, -1.382799517810166856, -14.66025672376848910 ) ) ;
#7790 = DIRECTION ( 'NONE',  ( 0.000000000000000000, -1.000000000000000000, 0.000000000000000000 ) ) ;
#7791 = VERTEX_POINT ( 'NONE', #16659 ) ;
#7792 =( NAMED_UNIT ( * ) PLANE_ANGLE_UNIT ( ) SI_UNIT ( $, .RADIAN. ) );
#7793 = AXIS2_PLACEMENT_3D ( 'NONE', #6563, #13000, #7997 ) ;
#7794 = CARTESIAN_POINT ( 'NONE',  ( 18.25624999999999787, 16.27314499999999953, 8.731249999999999289 ) ) ;
#7795 = DIRECTION ( 'NONE',  ( 0.9784543669157944601, 0.000000000000000000, 0.2064631973582987667 ) ) ;
#7796 = VERTEX_POINT ( 'NONE', #8131 ) ;
#7797 = LINE ( 'NONE', #21495, #7238 ) ;
#7798 = AXIS2_PLACEMENT_3D ( 'NONE', #11344, #15114, #2952 ) ;
#7799 = AXIS2_PLACEMENT_3D ( 'NONE', #18450, #13285, #13064 ) ;
#7800 = ORIENTED_EDGE ( 'NONE', *, *, #21503, .T. ) ;
#7801 = CARTESIAN_POINT ( 'NONE',  ( 11.06523579707593541, 17.51379554528373816, 6.791568276050612418 ) ) ;
#7802 = VECTOR ( 'NONE', #9794, 1000.000000000000000 ) ;
#7803 = ADVANCED_FACE ( 'NONE', ( #4500 ), #2839, .T. ) ;
#7804 = CARTESIAN_POINT ( 'NONE',  ( 6.020660706909825244, 11.11068921130002174, 1.355485640074744591 ) ) ;
#7805 = CARTESIAN_POINT ( 'NONE',  ( 20.09493269590303655, -3.218164174955788326, -15.32593859137127090 ) ) ;
#7806 = DIRECTION ( 'NONE',  ( 0.000000000000000000, -1.000000000000000000, 0.000000000000000000 ) ) ;
#7807 = VERTEX_POINT ( 'NONE', #8248 ) ;
#7808 = FACE_OUTER_BOUND ( 'NONE', #9524, .T. ) ;
#7809 =( GEOMETRIC_REPRESENTATION_CONTEXT ( 3 ) GLOBAL_UNCERTAINTY_ASSIGNED_CONTEXT ( ( #12116 ) ) GLOBAL_UNIT_ASSIGNED_CONTEXT ( ( #10539, #17177, #4128 ) ) REPRESENTATION_CONTEXT ( 'NONE', 'WORKASPACE' ) );
#7810 = VERTEX_POINT ( 'NONE', #11236 ) ;
#7811 = ORIENTED_EDGE ( 'NONE', *, *, #19425, .F. ) ;
#7812 = DIRECTION ( 'NONE',  ( -0.6287118719681975554, 0.000000000000000000, -0.7776383362760898033 ) ) ;
#7814 = DIRECTION ( 'NONE',  ( 0.7421532822901579785, 0.000000000000000000, -0.6702301885068630005 ) ) ;
#7813 = CARTESIAN_POINT ( 'NONE',  ( 2.298378135600148475, 19.81152135836902062, 0.4500434701621164879 ) ) ;
#7815 = ORIENTED_EDGE ( 'NONE', *, *, #2002, .T. ) ;
#7816 = CARTESIAN_POINT ( 'NONE',  ( 3.608170863617357504, 13.45129126140751019, -0.5713419425411067065 ) ) ;
#7817 = VERTEX_POINT ( 'NONE', #10017 ) ;
#7818 = ORIENTED_EDGE ( 'NONE', *, *, #1907, .F. ) ;
#7819 = CIRCLE ( 'NONE', #20503, 9.525000000000000355 ) ;
#7820 = ORIENTED_EDGE ( 'NONE', *, *, #12450, .T. ) ;
#7821 = VECTOR ( 'NONE', #2904, 1000.000000000000000 ) ;
#7822 = EDGE_CURVE ( 'NONE', #16730, #1384, #3063, .T. ) ;
#7823 = VECTOR ( 'NONE', #1120, 1000.000000000000000 ) ;
#7824 = VECTOR ( 'NONE', #4781, 1000.000000000000000 ) ;
#7825 = CARTESIAN_POINT ( 'NONE',  ( -0.8970842057359728061, 5.548947500000001476, -22.54358764576276286 ) ) ;
#7826 = CARTESIAN_POINT ( 'NONE',  ( 0.2641497867371597752, 5.548947500000001476, -24.43980549416641068 ) ) ;
#7827 = DIRECTION ( 'NONE',  ( -0.08192867786951699149, 0.000000000000000000, -0.9966381950048638361 ) ) ;
#7828 = DIRECTION ( 'NONE',  ( -0.3447671952293630548, 0.000000000000000000, -0.9386882235831439658 ) ) ;
#7829 = CARTESIAN_POINT ( 'NONE',  ( 3.622599477590417560, 16.21029899727770385, 9.208972499662912981 ) ) ;
#7830 = AXIS2_PLACEMENT_3D ( 'NONE', #8160, #14938, #1628 ) ;
#7831 = AXIS2_PLACEMENT_3D ( 'NONE', #13840, #3768, #10730 ) ;
#7832 = ORIENTED_EDGE ( 'NONE', *, *, #6921, .F. ) ;
#7833 = CARTESIAN_POINT ( 'NONE',  ( 42.66304184606194383, 42.06303499999999929, -19.22597499813143784 ) ) ;
#7834 = DIRECTION ( 'NONE',  ( 0.2490110332224850231, 0.000000000000000000, -0.9685006480810791629 ) ) ;
#7835 = DIRECTION ( 'NONE',  ( -2.876946610767471886E-14, 1.000000000000000000, 2.239739066241894173E-14 ) ) ;
#7836 =( NAMED_UNIT ( * ) PLANE_ANGLE_UNIT ( ) SI_UNIT ( $, .RADIAN. ) );
#7837 = FACE_OUTER_BOUND ( 'NONE', #13710, .T. ) ;
#7838 = ORIENTED_EDGE ( 'NONE', *, *, #9225, .F. ) ;
#7839 = VERTEX_POINT ( 'NONE', #7922 ) ;
#7840 = CARTESIAN_POINT ( 'NONE',  ( 9.598619977022886829, 11.43307009487834058, 0.5138147689867528234 ) ) ;
#7842 = DIRECTION ( 'NONE',  ( 0.2490110332224850509, 0.000000000000000000, -0.9685006480810792739 ) ) ;
#7841 = CARTESIAN_POINT ( 'NONE',  ( 10.02683081661366593, -14.84248999999999974, -16.89519978567464165 ) ) ;
#7843 = CARTESIAN_POINT ( 'NONE',  ( 12.08409848062061265, 21.36742032689186388, -1.692652775323916003 ) ) ;
#7844 = ORIENTED_EDGE ( 'NONE', *, *, #6729, .F. ) ;
#7845 = CIRCLE ( 'NONE', #11368, 0.5079999999999963434 ) ;
#7846 = VERTEX_POINT ( 'NONE', #14697 ) ;
#7847 = CARTESIAN_POINT ( 'NONE',  ( 39.16413618835606769, 32.54502000000000095, -24.45043885672975392 ) ) ;
#7848 = AXIS2_PLACEMENT_3D ( 'NONE', #16366, #21427, #1092 ) ;
#7849 = CARTESIAN_POINT ( 'NONE',  ( 8.223934500132745740, 20.88092512594423056, -0.6806936496286138949 ) ) ;
#7850 = CARTESIAN_POINT ( 'NONE',  ( 7.371918716459705756, 20.91752996184955293, 2.755765391713364210 ) ) ;
#7851 = VECTOR ( 'NONE', #1473, 1000.000000000000000 ) ;
#7852 = VECTOR ( 'NONE', #17743, 1000.000000000000000 ) ;
#7853 = EDGE_CURVE ( 'NONE', #7714, #8805, #21402, .T. ) ;
#7854 = DIRECTION ( 'NONE',  ( -0.9964481331860212121, 0.000000000000000000, 0.08420877549337302259 ) ) ;
#7855 = AXIS2_PLACEMENT_3D ( 'NONE', #10190, #13985, #3788 ) ;
#7856 = DIRECTION ( 'NONE',  ( -0.2490110332224850509, 0.000000000000000000, 0.9685006480810792739 ) ) ;
#7857 = CARTESIAN_POINT ( 'NONE',  ( 52.91086381164393515, 0.000000000000000000, 3.812938856729753301 ) ) ;
#7858 = CARTESIAN_POINT ( 'NONE',  ( 46.03750000000000142, 32.54502000000000095, -10.31874999999999964 ) ) ;
#7859 = CARTESIAN_POINT ( 'NONE',  ( 1.679183762215729736, 14.29506049579505067, 9.182897261660000865 ) ) ;
#7860 = ORIENTED_EDGE ( 'NONE', *, *, #13177, .T. ) ;
#7861 = CARTESIAN_POINT ( 'NONE',  ( 5.607325312162852349, 20.83420574847494322, 3.738502895875575938 ) ) ;
#7862 = CARTESIAN_POINT ( 'NONE',  ( -1.351150467732365579, 26.98019749999999917, -27.17319717629097653 ) ) ;
#7863 = DIRECTION ( 'NONE',  ( -0.6702301885068632226, 0.000000000000000000, -0.7421532822901576454 ) ) ;
#7864 = CARTESIAN_POINT ( 'NONE',  ( 14.56022883136782298, -8.303717150559636551, -15.17570085620177878 ) ) ;
#7865 = VERTEX_POINT ( 'NONE', #21626 ) ;
#7866 = CARTESIAN_POINT ( 'NONE',  ( 45.99559936598748777, 32.54502000000000095, 5.449572532947073000 ) ) ;
#7867 = AXIS2_PLACEMENT_3D ( 'NONE', #11001, #10791, #17536 ) ;
#7868 = CARTESIAN_POINT ( 'NONE',  ( 9.163832593674008820, 13.38766655458928767, -2.811206270904612836 ) ) ;
#7869 = ORIENTED_EDGE ( 'NONE', *, *, #12821, .F. ) ;
#7870 = CARTESIAN_POINT ( 'NONE',  ( 27.93851334206399883, 1.396555486991390094, 10.62689512540016068 ) ) ;
#7871 = CARTESIAN_POINT ( 'NONE',  ( 7.990381836082426581, 21.45420684216762908, 4.447820836819799339 ) ) ;
#7872 = CARTESIAN_POINT ( 'NONE',  ( 9.907371917564091746, -3.968114999999999615, -13.23786778167655243 ) ) ;
#7873 = CARTESIAN_POINT ( 'NONE',  ( 3.365948022932646833, 20.63951482243974311, 3.619662730472012147 ) ) ;
#7874 = VERTEX_POINT ( 'NONE', #18101 ) ;
#7875 = ITEM_DEFINED_TRANSFORMATION ( 'NONE', 'NONE', #6995,  #2234 ) ;
#7876 = EDGE_CURVE ( 'NONE', #19395, #5980, #13127, .T. ) ;
#7877 = DIRECTION ( 'NONE',  ( 0.9980811434661737147, 0.000000000000000000, 0.06191955310929838502 ) ) ;
#7878 = CIRCLE ( 'NONE', #18114, 0.5079999999999995630 ) ;
#7879 = CARTESIAN_POINT ( 'NONE',  ( 21.03437500000000071, 32.54502000000000095, 5.159374999999999822 ) ) ;
#7880 = EDGE_CURVE ( 'NONE', #7705, #3294, #21572, .T. ) ;
#7881 = VECTOR ( 'NONE', #17492, 1000.000000000000000 ) ;
#7882 = CARTESIAN_POINT ( 'NONE',  ( 10.61004938962564026, 20.41586353969747947, 4.879409801239452449 ) ) ;
#7883 = EDGE_CURVE ( 'NONE', #1876, #7573, #20499, .T. ) ;
#7884 = CARTESIAN_POINT ( 'NONE',  ( 5.236457354293306388, 17.24636926302095929, 7.945963056083468423 ) ) ;
#7885 = CARTESIAN_POINT ( 'NONE',  ( 3.733050171586274502, 21.36287299093768155, 3.432506848783466236 ) ) ;
#7886 = DIRECTION ( 'NONE',  ( -0.9685006480810792739, 0.000000000000000000, -0.2490110332224850231 ) ) ;
#7887 = CARTESIAN_POINT ( 'NONE',  ( 32.18388890846549799, 0.000000000000000000, 1.507793899792891468 ) ) ;
#7888 = CARTESIAN_POINT ( 'NONE',  ( 6.767696032117554772, 11.35695232375848107, 2.710251460945410251 ) ) ;
#7889 = CARTESIAN_POINT ( 'NONE',  ( 20.07682953892606648, -1.527641563098319333, -15.89113342295757292 ) ) ;
#7890 = CYLINDRICAL_SURFACE ( 'NONE', #20535, 0.7950200000000005041 ) ;
#7891 = CIRCLE ( 'NONE', #15687, 1.984374999999999112 ) ;
#7892 = CYLINDRICAL_SURFACE ( 'NONE', #12751, 6.349999999999997868 ) ;
#7893 = ORIENTED_EDGE ( 'NONE', *, *, #18410, .T. ) ;
#7894 = DIRECTION ( 'NONE',  ( 0.000000000000000000, 1.000000000000000000, 0.000000000000000000 ) ) ;
#7895 = LINE ( 'NONE', #16318, #11543 ) ;
#7896 = ORIENTED_EDGE ( 'NONE', *, *, #10159, .T. ) ;
#7897 = CARTESIAN_POINT ( 'NONE',  ( 9.518858328804567392, 18.01013026545717111, -2.601155476716757509 ) ) ;
#7898 = CARTESIAN_POINT ( 'NONE',  ( 0.6624797471569731089, 19.52062711105720894, 7.302438800931884799 ) ) ;
#7899 = CARTESIAN_POINT ( 'NONE',  ( 14.17791483913661388, -8.465630425894779876, -16.51628623702010401 ) ) ;
#7900 = LINE ( 'NONE', #6345, #11702 ) ;
#7901 = VERTEX_POINT ( 'NONE', #11674 ) ;
#7902 = EDGE_CURVE ( 'NONE', #1582, #14783, #17707, .T. ) ;
#7903 = DIRECTION ( 'NONE',  ( -0.8609107660235848503, 0.000000000000000000, 0.5087559856598096175 ) ) ;
#7904 = PRODUCT_RELATED_PRODUCT_CATEGORY ( 'part', '', ( #18165 ) ) ;
#7905 = ORIENTED_EDGE ( 'NONE', *, *, #9789, .T. ) ;
#7906 = CARTESIAN_POINT ( 'NONE',  ( 19.94878033733339606, -0.9245715916927551570, -14.84082521870049476 ) ) ;
#7907 = CARTESIAN_POINT ( 'NONE',  ( 0.6071489226691182406, 19.09056084336265613, 1.779463758861457023 ) ) ;
#7908 = CIRCLE ( 'NONE', #20964, 0.5080000000000023386 ) ;
#7909 = B_SPLINE_SURFACE_WITH_KNOTS ( 'NONE', 3, 3, ( 
 ( #2502, #2616, #10692, #12577, #10800, #2397, #17440, #5587, #21066, #2280, #9236, #19300, #7367, #4058, #9347, #9018, #19194, #4162, #730 ),
 ( #5917, #11123, #21172, #6030, #2721, #15794, #7267, #10904, #4389, #17875, #16016, #623, #4277, #17546, #5821, #17653, #14137, #15688, #7591 ),
 ( #19524, #515, #14027, #11014, #20839, #20732, #845, #15905, #12348, #947, #7480, #19073, #3948, #14351, #7694, #14249, #16117, #5710, #12680 ),
 ( #19404, #12468, #9125, #14455, #20966, #17770, #6578, #1273, #19948, #20044, #16332, #11340, #4915, #2947, #16543, #18396, #18201, #13342, #21726 ),
 ( #16226, #8016, #6355, #14573, #14685, #19839, #11227, #1170, #7910, #18295, #21392, #9675, #16443, #4714, #8117, #6245, #21497, #9878, #13239 ),
 ( #14897, #6475, #16644, #1489, #8236, #15009, #15329, #6680, #18610, #20474, #13661, #10327, #8661, #17180, #262, #7125, #5024, #5343, #20593 ),
 ( #18508, #15109, #12215, #10107, #3271, #21828, #1697, #13442, #16093, #20704, #14107, #4133, #17517, #2253, #9204, #17288, #15661, #14002, #5559 ),
 ( #12317, #10874, #10664, #15770, #2475, #20810, #7563, #12440, #2366, #16239, #12693, #6370, #11240, #2963, #9689, #19313, #16455, #14702, #14363 ),
 ( #4503, #19540, #1291, #4611, #11139, #14805, #10918, #1069, #11356, #17887, #19737, #19417, #7708, #5929, #21079, #21405, #6161, #2520, #4291 ) ),
 .UNSPECIFIED., .F., .F., .F.,
 ( 4, 1, 1, 1, 1, 1, 4 ),
 ( 4, 1, 1, 1, 1, 1, 1, 1, 1, 1, 1, 1, 1, 1, 1, 1, 4 ),
 ( -0.01351613576970000022, 0.000000000000000000, 0.1250000000000000000, 0.2500000000000000000, 0.3750000000000000000, 0.5000000000000000000, 0.5135161357697000106 ),
 ( -0.02000000026063999958, 0.04500000058643999906, 0.1100000014334999998, 0.1750000022806000033, 0.2400000031276999790, 0.3050000039747000069, 0.3700000048218000104, 0.4350000056689000139, 0.5000000065160000728, 0.5650000073629999342, 0.6300000082101000487, 0.6950000090572000522, 0.7600000099042999446, 0.8250000107513000280, 0.8900000115984000315, 0.9550000124454999240, 1.020000013293000052 ),
 .UNSPECIFIED. ) ;
#7910 = CARTESIAN_POINT ( 'NONE',  ( 12.01347082551317769, -0.1802273000781166867, -17.35803166960114652 ) ) ;
#7911 = ORIENTED_EDGE ( 'NONE', *, *, #18950, .F. ) ;
#7912 = CARTESIAN_POINT ( 'NONE',  ( 12.39952505252417225, 11.21852838486178250, 2.567359074515783934 ) ) ;
#7913 = EDGE_CURVE ( 'NONE', #17335, #9687, #9894, .T. ) ;
#7914 = CARTESIAN_POINT ( 'NONE',  ( 2.846561112771937463, 19.99446726697395604, 2.016362468292247634 ) ) ;
#7915 = CARTESIAN_POINT ( 'NONE',  ( 38.24394060764427650, 39.20076311267237656, -4.842470972476202284 ) ) ;
#7916 = CARTESIAN_POINT ( 'NONE',  ( 12.45929919478725978, 10.42866963796318025, 2.734625762110018954 ) ) ;
#7917 = VECTOR ( 'NONE', #7721, 1000.000000000000000 ) ;
#7918 = CARTESIAN_POINT ( 'NONE',  ( 19.52926446840631769, -5.159662720637996358, -15.37549714948907287 ) ) ;
#7919 = DIRECTION ( 'NONE',  ( 0.9636276526537417286, 0.000000000000000000, -0.2672484743474499158 ) ) ;
#7920 = ORIENTED_EDGE ( 'NONE', *, *, #21653, .F. ) ;
#7921 = DIRECTION ( 'NONE',  ( 0.000000000000000000, 1.000000000000000000, 0.000000000000000000 ) ) ;
#7922 = CARTESIAN_POINT ( 'NONE',  ( 38.60701496492545459, 32.54502000000000095, -26.94161103631838472 ) ) ;
#7923 = AXIS2_PLACEMENT_3D ( 'NONE', #16205, #9100, #602 ) ;
#7924 = ORIENTED_EDGE ( 'NONE', *, *, #17072, .T. ) ;
#7925 = ORIENTED_EDGE ( 'NONE', *, *, #19281, .F. ) ;
#7926 = DIRECTION ( 'NONE',  ( -0.6702301885068652210, 0.000000000000000000, -0.7421532822901560911 ) ) ;
#7928 = CARTESIAN_POINT ( 'NONE',  ( 1.268730000000000135, 9.129395000000000593, 8.609509071587499562 ) ) ;
#7927 = CARTESIAN_POINT ( 'NONE',  ( 1.776609477927864944, 21.29427857361828202, 5.019511698632141083 ) ) ;
#7929 = ORIENTED_EDGE ( 'NONE', *, *, #4219, .F. ) ;
#7930 = CARTESIAN_POINT ( 'NONE',  ( 4.453886262617038128, 20.54954622212565951, 0.5777918640390905525 ) ) ;
#7931 = EDGE_CURVE ( 'NONE', #10813, #19794, #7109, .T. ) ;
#7932 = VERTEX_POINT ( 'NONE', #18522 ) ;
#7933 = EDGE_CURVE ( 'NONE', #7932, #19746, #8494, .T. ) ;
#7934 = ORIENTED_EDGE ( 'NONE', *, *, #20016, .F. ) ;
#7935 = CIRCLE ( 'NONE', #11825, 0.7950199999999993938 ) ;
#7936 = CARTESIAN_POINT ( 'NONE',  ( 0.7908948794667333138, 12.21508164119194539, 4.984945765070319723 ) ) ;
#7937 = VERTEX_POINT ( 'NONE', #1712 ) ;
#7938 = CARTESIAN_POINT ( 'NONE',  ( 2.434666203727371858, 12.17329066828716755, 3.243477976185151324 ) ) ;
#7939 = VECTOR ( 'NONE', #13293, 1000.000000000000114 ) ;
#7940 = CARTESIAN_POINT ( 'NONE',  ( 52.49113927203449492, -6.356984999999999886, -16.14695822742181619 ) ) ;
#7941 = CARTESIAN_POINT ( 'NONE',  ( -12.30312499999999964, 2.380615000000000148, 8.731249999999999289 ) ) ;
#7942 = LINE ( 'NONE', #12831, #1195 ) ;
#7943 = DIRECTION ( 'NONE',  ( -0.9966381950048638361, 0.000000000000000000, 0.08192867786951606168 ) ) ;
#7944 = CARTESIAN_POINT ( 'NONE',  ( 2.901118926289983690, 11.36639711562255961, 5.314311948376294836 ) ) ;
#7945 = VERTEX_POINT ( 'NONE', #8864 ) ;
#7946 = CARTESIAN_POINT ( 'NONE',  ( 1.954387715434429795, 9.129395000000000593, 6.745605000000000295 ) ) ;
#7947 = CARTESIAN_POINT ( 'NONE',  ( 65.64431122251959039, 1.984375000000000000, -11.29787305743958115 ) ) ;
#7948 = CARTESIAN_POINT ( 'NONE',  ( 13.08245519309633309, 21.51426585157789972, 1.947758980082396896 ) ) ;
#7949 = DIRECTION ( 'NONE',  ( 0.9822019212503901864, 0.000000000000000000, -0.1878280753562740768 ) ) ;
#7950 = CARTESIAN_POINT ( 'NONE',  ( 53.76119506325677122, 39.48900909932986281, -15.89313734090458397 ) ) ;
#7951 = ORIENTED_EDGE ( 'NONE', *, *, #18149, .T. ) ;
#7952 = ORIENTED_EDGE ( 'NONE', *, *, #468, .F. ) ;
#7953 = CARTESIAN_POINT ( 'NONE',  ( 8.345656034557093150, 19.69124030533750158, 6.193199096954582927 ) ) ;
#7955 = CYLINDRICAL_SURFACE ( 'NONE', #18417, 30.16249999999999076 ) ;
#7954 = PLANE ( 'NONE',  #17552 ) ;
#7956 = CARTESIAN_POINT ( 'NONE',  ( 11.06000417728166418, 12.98885560605806688, -3.324977026302950556 ) ) ;
#7957 = ORIENTED_EDGE ( 'NONE', *, *, #8999, .T. ) ;
#7958 = CIRCLE ( 'NONE', #183, 0.7950200000000000600 ) ;
#7959 = VERTEX_POINT ( 'NONE', #8451 ) ;
#7960 = EDGE_CURVE ( 'NONE', #5639, #14728, #19153, .T. ) ;
#7961 = LINE ( 'NONE', #1427, #3555 ) ;
#7962 = CARTESIAN_POINT ( 'NONE',  ( 8.191486769309802796, 20.38885208666888005, 4.925509210000734051 ) ) ;
#7963 = CARTESIAN_POINT ( 'NONE',  ( 6.964527527572196952, 12.34030082466796863, 5.404614456109265497 ) ) ;
#7964 = AXIS2_PLACEMENT_3D ( 'NONE', #18590, #7103, #1898 ) ;
#7965 = DIRECTION ( 'NONE',  ( 0.000000000000000000, 1.000000000000000000, 0.000000000000000000 ) ) ;
#7966 = DIRECTION ( 'NONE',  ( 0.6496772031432432870, 0.000000000000000000, -0.7602101891687411683 ) ) ;
#7967 = FACE_BOUND ( 'NONE', #21837, .T. ) ;
#7968 = CARTESIAN_POINT ( 'NONE',  ( 1.134328099840657966, 11.72196338839733265, 6.483094573881109213 ) ) ;
#7969 = CARTESIAN_POINT ( 'NONE',  ( 54.51779242482700027, 30.56064500000000095, -30.64740209392260084 ) ) ;
#7970 = ORIENTED_EDGE ( 'NONE', *, *, #15268, .T. ) ;
#7971 = CARTESIAN_POINT ( 'NONE',  ( 6.291547558928166417, 11.65658372465740200, 2.472496458133855768 ) ) ;
#7972 = DIRECTION ( 'NONE',  ( -0.9959941601142525691, 0.000000000000000000, -0.08941830359777946935 ) ) ;
#7973 = CARTESIAN_POINT ( 'NONE',  ( 11.42842559562532578, 34.52875999999999834, 1.673196738795719174 ) ) ;
#7974 = CARTESIAN_POINT ( 'NONE',  ( 15.68359214062586560, -8.436795285945176914, -14.92921296275496701 ) ) ;
#7975 = ORIENTED_EDGE ( 'NONE', *, *, #4022, .F. ) ;
#7976 = DIRECTION ( 'NONE',  ( 0.05085730733808142834, 0.000000000000000000, -0.9987059298363657467 ) ) ;
#7977 = CARTESIAN_POINT ( 'NONE',  ( 10.69351799873146902, 10.89466173679246097, 4.203936836416402478 ) ) ;
#7978 = CARTESIAN_POINT ( 'NONE',  ( 9.437281383587103889, 11.84308063076154660, -1.503547281869039853 ) ) ;
#7979 = ORIENTED_EDGE ( 'NONE', *, *, #37, .F. ) ;
#7980 = CARTESIAN_POINT ( 'NONE',  ( 29.36887348155339694, 1.984374998761125219, 10.71562877576799977 ) ) ;
#7981 = ADVANCED_FACE ( 'NONE', ( #17277 ), #18924, .T. ) ;
#7982 = CARTESIAN_POINT ( 'NONE',  ( 11.69496188115748048, 19.47354328404300716, -2.596091651573762427 ) ) ;
#7983 = CARTESIAN_POINT ( 'NONE',  ( 7.241256223353114585, 21.68187987146653128, 2.393131185843784703 ) ) ;
#7984 = CARTESIAN_POINT ( 'NONE',  ( 36.80301088673436283, -1.983739999999999837, -23.10021947667301134 ) ) ;
#7985 = CARTESIAN_POINT ( 'NONE',  ( 5.888945687064545353, 12.28013972695870137, 0.9976771953365630718 ) ) ;
#7986 = SURFACE_STYLE_FILL_AREA ( #14425 ) ;
#7987 = LINE ( 'NONE', #14863, #12527 ) ;
#7988 = CARTESIAN_POINT ( 'NONE',  ( 6.247512289571992561, 18.85032048260596227, -1.008565764037584023 ) ) ;
#7989 = FACE_OUTER_BOUND ( 'NONE', #8790, .T. ) ;
#7990 = CARTESIAN_POINT ( 'NONE',  ( 1.243233153551759784, 11.63297050342826289, 6.525882853348925927 ) ) ;
#7991 = LINE ( 'NONE', #1463, #4712 ) ;
#7992 = DIRECTION ( 'NONE',  ( 0.000000000000000000, 1.000000000000000000, -0.000000000000000000 ) ) ;
#7993 = CARTESIAN_POINT ( 'NONE',  ( 6.680663975448227987, 11.57849123843430128, 2.752492323310664180 ) ) ;
#7994 = CARTESIAN_POINT ( 'NONE',  ( 52.94935177953276195, 40.07877905746412495, -16.57402588728236381 ) ) ;
#7995 = EDGE_CURVE ( 'NONE', #10315, #21656, #20689, .T. ) ;
#7996 = FACE_OUTER_BOUND ( 'NONE', #17675, .T. ) ;
#7997 = DIRECTION ( 'NONE',  ( -0.7532174416907910786, 0.000000000000000000, -0.6577716059034319773 ) ) ;
#7998 = VERTEX_POINT ( 'NONE', #3795 ) ;
#7999 = CARTESIAN_POINT ( 'NONE',  ( 45.99559936598748777, 0.000000000000000000, 5.449572532947073000 ) ) ;
#8000 = CARTESIAN_POINT ( 'NONE',  ( -4.728951812473551897, 28.56769750000000130, -29.02782796843600011 ) ) ;
#8001 = ORIENTED_EDGE ( 'NONE', *, *, #4912, .F. ) ;
#8002 = EDGE_CURVE ( 'NONE', #21819, #3005, #5684, .T. ) ;
#8003 = CARTESIAN_POINT ( 'NONE',  ( 12.29938047911826438, 20.21572945018251843, 4.621882145428052979 ) ) ;
#8004 = FACE_OUTER_BOUND ( 'NONE', #18550, .T. ) ;
#8005 = CARTESIAN_POINT ( 'NONE',  ( 52.98023334790573102, 37.69393439911831933, -16.84172433709920469 ) ) ;
#8006 = EDGE_CURVE ( 'NONE', #7817, #8727, #14207, .T. ) ;
#8007 = CARTESIAN_POINT ( 'NONE',  ( 20.50355652906860371, -2.693653029022725853, -13.33117366251859082 ) ) ;
#8008 = CARTESIAN_POINT ( 'NONE',  ( 46.03750000000000142, 1.984375000000000000, -10.31874999999999964 ) ) ;
#8009 = ORIENTED_EDGE ( 'NONE', *, *, #12944, .T. ) ;
#8010 = CARTESIAN_POINT ( 'NONE',  ( 0.000000000000000000, 0.000000000000000000, 0.000000000000000000 ) ) ;
#8011 = DIRECTION ( 'NONE',  ( 0.8334497143791951279, 0.000000000000000000, 0.5525953072558960066 ) ) ;
#8012 = CARTESIAN_POINT ( 'NONE',  ( 3.870040991641794381, 17.28388692985063102, -0.5782205561518194425 ) ) ;
#8013 = ORIENTED_EDGE ( 'NONE', *, *, #18142, .T. ) ;
#8014 = CARTESIAN_POINT ( 'NONE',  ( 19.72907204108386381, -0.5191967632752201300, -14.91740567612944623 ) ) ;
#8015 = CARTESIAN_POINT ( 'NONE',  ( 0.7706404128728925329, 19.48544532655929729, 2.171001955729903177 ) ) ;
#8016 = CARTESIAN_POINT ( 'NONE',  ( 20.65797006290371840, -1.382799537871407747, -15.93813883736856418 ) ) ;
#8017 = ORIENTED_EDGE ( 'NONE', *, *, #5836, .F. ) ;
#8018 = CARTESIAN_POINT ( 'NONE',  ( 5.585406168101782143, 13.98417111045325001, -0.8546884854210520244 ) ) ;
#8019 = CARTESIAN_POINT ( 'NONE',  ( 38.36548343274824902, 39.62000810270092188, -4.672696708993173687 ) ) ;
#8020 = CARTESIAN_POINT ( 'NONE',  ( 12.92989047915411582, 22.29005399844394120, 0.3614750032390292578 ) ) ;
#8021 = VECTOR ( 'NONE', #4859, 1000.000000000000000 ) ;
#8022 = ADVANCED_FACE ( 'NONE', ( #10531 ), #20162, .T. ) ;
#8023 = ORIENTED_EDGE ( 'NONE', *, *, #20136, .T. ) ;
#8024 = DIRECTION ( 'NONE',  ( 0.000000000000000000, -1.000000000000000000, -0.000000000000000000 ) ) ;
#8025 = CARTESIAN_POINT ( 'NONE',  ( 19.79515554403045741, -1.983739999999999393, -10.69562145279641996 ) ) ;
#8026 = VERTEX_POINT ( 'NONE', #10863 ) ;
#8027 = EDGE_LOOP ( 'NONE', ( #15902, #9560, #7273, #18680 ) ) ;
#8028 = CARTESIAN_POINT ( 'NONE',  ( 44.28293121686854761, -3.968114999999999615, -31.08068102505560759 ) ) ;
#8029 = EDGE_CURVE ( 'NONE', #10927, #10511, #15238, .T. ) ;
#8031 = CARTESIAN_POINT ( 'NONE',  ( 50.52547294529469468, 38.88803500000000213, -18.64987929725020521 ) ) ;
#8030 = CARTESIAN_POINT ( 'NONE',  ( 6.634819837061233905, 10.91373323652594252, 4.277435202800065284 ) ) ;
#8032 = ORIENTED_EDGE ( 'NONE', *, *, #8006, .F. ) ;
#8033 = CARTESIAN_POINT ( 'NONE',  ( 3.778158909772205476, 12.44086029795262505, 0.2773760682544378908 ) ) ;
#8034 = ORIENTED_EDGE ( 'NONE', *, *, #5527, .T. ) ;
#8035 = VECTOR ( 'NONE', #12481, 1000.000000000000227 ) ;
#8036 = ORIENTED_EDGE ( 'NONE', *, *, #13314, .F. ) ;
#8037 = CARTESIAN_POINT ( 'NONE',  ( 0.6379514360146986141, 12.25052848803336758, 4.278287073605215873 ) ) ;
#8038 = ORIENTED_EDGE ( 'NONE', *, *, #21688, .F. ) ;
#8039 = CARTESIAN_POINT ( 'NONE',  ( 2.515435776023313696, 12.09851621675084665, 3.613288693446259803 ) ) ;
#8040 = CARTESIAN_POINT ( 'NONE',  ( 4.151218630365011819, 12.29860231867225728, 1.847275165616512949 ) ) ;
#8041 = CARTESIAN_POINT ( 'NONE',  ( 50.62387473582167274, 32.54502000000000095, -28.41576006634952734 ) ) ;
#8042 = EDGE_CURVE ( 'NONE', #18076, #12952, #12423, .T. ) ;
#8043 = CARTESIAN_POINT ( 'NONE',  ( 44.27024749654656688, 38.88803500000000213, -8.722764363618033201 ) ) ;
#8044 = DIRECTION ( 'NONE',  ( -0.2868778675745011220, 0.000000000000000000, -0.9579671649362034858 ) ) ;
#8045 = CARTESIAN_POINT ( 'NONE',  ( 3.605855464307719860, 16.44159216467194540, 9.204281209079420378 ) ) ;
#8046 = EDGE_CURVE ( 'NONE', #9688, #539, #10121, .T. ) ;
#8047 = EDGE_CURVE ( 'NONE', #9687, #3268, #5983, .T. ) ;
#8048 = VECTOR ( 'NONE', #4001, 1000.000000000000114 ) ;
#8049 = ORIENTED_EDGE ( 'NONE', *, *, #1460, .F. ) ;
#8050 = CARTESIAN_POINT ( 'NONE',  ( 30.97944403357121956, 0.000000000000000000, -8.103300075789407586 ) ) ;
#8051 = DIRECTION ( 'NONE',  ( 0.000000000000000000, 1.000000000000000000, 0.000000000000000000 ) ) ;
#8052 = CARTESIAN_POINT ( 'NONE',  ( 13.13545844809530116, 21.45922784306827324, 1.923808864204277658 ) ) ;
#8053 = DIRECTION ( 'NONE',  ( 0.000000000000000000, 1.000000000000000000, 0.000000000000000000 ) ) ;
#8054 = ORIENTED_EDGE ( 'NONE', *, *, #6411, .T. ) ;
#8055 = ORIENTED_EDGE ( 'NONE', *, *, #16264, .T. ) ;
#8056 = CARTESIAN_POINT ( 'NONE',  ( 11.01329100639444825, 21.44411105555546015, 2.081521072878112832 ) ) ;
#8057 = PRODUCT_DEFINITION_FORMATION_WITH_SPECIFIED_SOURCE ( 'ANY', '', #19722, .NOT_KNOWN. ) ;
#8058 = CYLINDRICAL_SURFACE ( 'NONE', #17913, 1.190624999999999822 ) ;
#8059 = CARTESIAN_POINT ( 'NONE',  ( 11.16145234711147793, 18.34406730449142842, -4.030487463324528896 ) ) ;
#8060 = ORIENTED_EDGE ( 'NONE', *, *, #13327, .F. ) ;
#8061 = ORIENTED_EDGE ( 'NONE', *, *, #9791, .T. ) ;
#8062 = CARTESIAN_POINT ( 'NONE',  ( 53.25483508941461963, 34.52875999999999834, -5.879799058943532941 ) ) ;
#8063 = CARTESIAN_POINT ( 'NONE',  ( 8.300069718050908207, 11.53897452521841061, 2.298314304733178659 ) ) ;
#8064 = VECTOR ( 'NONE', #2390, 1000.000000000000114 ) ;
#8065 = CARTESIAN_POINT ( 'NONE',  ( 2.899589520589617830, 18.93284891393944847, 7.571049628500222006 ) ) ;
#8066 = FACE_OUTER_BOUND ( 'NONE', #10665, .T. ) ;
#8067 = CYLINDRICAL_SURFACE ( 'NONE', #15545, 1.190624999999999822 ) ;
#8068 = CARTESIAN_POINT ( 'NONE',  ( 1.642651581313985920, 16.44733452758824654, -0.7885569526307778521 ) ) ;
#8069 = CARTESIAN_POINT ( 'NONE',  ( 0.8410692468848214309, 11.43456274839658349, 5.196488955505333074 ) ) ;
#8070 = EDGE_CURVE ( 'NONE', #21386, #4038, #1558, .T. ) ;
#8071 = CARTESIAN_POINT ( 'NONE',  ( 28.97711086133420366, 32.54502000000000095, -10.31874999999999964 ) ) ;
#8072 = ORIENTED_EDGE ( 'NONE', *, *, #7088, .F. ) ;
#8073 = CARTESIAN_POINT ( 'NONE',  ( 3.927156886961982174, 12.81957249642222152, 0.8896893740454994148 ) ) ;
#8074 = FACE_OUTER_BOUND ( 'NONE', #1390, .T. ) ;
#8075 = DIRECTION ( 'NONE',  ( 0.000000000000000000, -1.000000000000000000, 0.000000000000000000 ) ) ;
#8076 = CARTESIAN_POINT ( 'NONE',  ( 5.430521817098937554, -1.594802499999999013, -21.76500205408690647 ) ) ;
#8077 = ORIENTED_EDGE ( 'NONE', *, *, #419, .F. ) ;
#8078 = CARTESIAN_POINT ( 'NONE',  ( 11.08364749134637783, 12.02016517962410269, 5.901226234691837824 ) ) ;
#8079 = CIRCLE ( 'NONE', #20414, 0.3962400000000010358 ) ;
#8080 = DIRECTION ( 'NONE',  ( -0.7421532822901579785, 0.000000000000000000, 0.6702301885068630005 ) ) ;
#8081 = CARTESIAN_POINT ( 'NONE',  ( 9.075132670590440043, 14.78225112982097222, -3.399159583193371414 ) ) ;
#8082 = EDGE_LOOP ( 'NONE', ( #2656, #19743, #13384, #2849, #19189, #4840 ) ) ;
#8083 = CARTESIAN_POINT ( 'NONE',  ( 6.671004511676491333, 21.25262578982561124, 0.8364515325576188376 ) ) ;
#8084 = LINE ( 'NONE', #16506, #14136 ) ;
#8085 = CARTESIAN_POINT ( 'NONE',  ( 2.523890540482722766, 12.01182523388594170, 3.570307163362016922 ) ) ;
#8086 = AXIS2_PLACEMENT_3D ( 'NONE', #7984, #4467, #1247 ) ;
#8087 = CARTESIAN_POINT ( 'NONE',  ( 29.36874999999999858, 22.62187499999999929, 8.731249999999999289 ) ) ;
#8088 = DIRECTION ( 'NONE',  ( 0.1060008583745224581, 0.000000000000000000, 0.9943660382494288186 ) ) ;
#8089 = AXIS2_PLACEMENT_3D ( 'NONE', #10677, #14014, #2601 ) ;
#8090 = CARTESIAN_POINT ( 'NONE',  ( 13.51825059216985103, 14.85126536588636981, 6.305477837050446510 ) ) ;
#8091 = CARTESIAN_POINT ( 'NONE',  ( 5.937100890138371057, 21.55539096890324302, 3.690821903281856553 ) ) ;
#8092 = CARTESIAN_POINT ( 'NONE',  ( 1.445847263472733291, 34.12394749999999988, -6.267054683493481271 ) ) ;
#8093 = EDGE_CURVE ( 'NONE', #513, #18859, #18357, .T. ) ;
#8094 = PLANE ( 'NONE',  #71 ) ;
#8095 = CARTESIAN_POINT ( 'NONE',  ( 6.736892714481453659, 11.48351050777079330, 2.728717353481319385 ) ) ;
#8096 = DIRECTION ( 'NONE',  ( 0.6287118719681975554, 0.000000000000000000, 0.7776383362760898033 ) ) ;
#8097 = CYLINDRICAL_SURFACE ( 'NONE', #13161, 0.7950200000000003930 ) ;
#8098 = CARTESIAN_POINT ( 'NONE',  ( 40.21953902438700368, -6.356984999999999886, -3.460331122294329820 ) ) ;
#8099 = ORIENTED_EDGE ( 'NONE', *, *, #11131, .T. ) ;
#8100 = CARTESIAN_POINT ( 'NONE',  ( 30.78626241496060700, 38.48766750000000059, -2.552201779827368622 ) ) ;
#8101 = EDGE_CURVE ( 'NONE', #13851, #13712, #2884, .T. ) ;
#8102 = CARTESIAN_POINT ( 'NONE',  ( 10.10534066920194185, -95.96551800000000298, -14.00784516691476966 ) ) ;
#8103 = VERTEX_POINT ( 'NONE', #3440 ) ;
#8104 = CARTESIAN_POINT ( 'NONE',  ( 13.05080356390050156, 13.28370079963820771, 5.434073716250534147 ) ) ;
#8105 = DIRECTION ( 'NONE',  ( 0.2490110332224850509, 0.000000000000000000, -0.9685006480810792739 ) ) ;
#8106 = CARTESIAN_POINT ( 'NONE',  ( 12.76235139282079167, 21.25996874134203907, -20.69948241803004407 ) ) ;
#8107 = CARTESIAN_POINT ( 'NONE',  ( 19.52298845727983689, -0.8684148934049937818, -15.62363129117676941 ) ) ;
#8108 = CARTESIAN_POINT ( 'NONE',  ( 46.03750000000000142, 42.06303499999999929, -10.31874999999999964 ) ) ;
#8109 = VERTEX_POINT ( 'NONE', #16918 ) ;
#8110 = DIRECTION ( 'NONE',  ( 0.000000000000000000, 0.000000000000000000, 1.000000000000000000 ) ) ;
#8111 = CARTESIAN_POINT ( 'NONE',  ( 6.016625000000000334, 32.54502000000000095, 2.794000000000000039 ) ) ;
#8112 = ORIENTED_EDGE ( 'NONE', *, *, #52, .T. ) ;
#8113 = CIRCLE ( 'NONE', #10229, 1.785937499999998179 ) ;
#8114 = CARTESIAN_POINT ( 'NONE',  ( 19.75485755962498757, -0.5674586355576572982, -14.90795299099519511 ) ) ;
#8115 = CARTESIAN_POINT ( 'NONE',  ( 0.2522477005385261872, 17.74294589129466715, 1.020296498861633427 ) ) ;
#8116 = AXIS2_PLACEMENT_3D ( 'NONE', #16863, #7137, #13906 ) ;
#8117 = CARTESIAN_POINT ( 'NONE',  ( 17.85758357290024634, -7.713152382332621571, -15.13302928010427273 ) ) ;
#8118 = VERTEX_POINT ( 'NONE', #19909 ) ;
#8119 = CARTESIAN_POINT ( 'NONE',  ( 10.27701911607673679, 11.26312240063166037, 2.186809789112166058 ) ) ;
#8120 = DIRECTION ( 'NONE',  ( -0.9767031480033347979, 0.000000000000000000, 0.2145948757085687775 ) ) ;
#8121 = CARTESIAN_POINT ( 'NONE',  ( 8.612298605082777669, 10.74346438930206027, 3.697136140246361613 ) ) ;
#8122 = ADVANCED_FACE ( 'NONE', ( #11511 ), #11739, .F. ) ;
#8123 = VECTOR ( 'NONE', #15838, 1000.000000000000227 ) ;
#8124 = ADVANCED_FACE ( 'NONE', ( #15290 ), #3223, .F. ) ;
#8125 = CARTESIAN_POINT ( 'NONE',  ( 18.19505925514423339, -6.585633048537570033, -15.62533351450368002 ) ) ;
#8126 = FACE_OUTER_BOUND ( 'NONE', #10582, .T. ) ;
#8127 = ORIENTED_EDGE ( 'NONE', *, *, #7933, .T. ) ;
#8128 = CIRCLE ( 'NONE', #4606, 0.5080000000000002292 ) ;
#8129 = CARTESIAN_POINT ( 'NONE',  ( 8.599976436249926692, 20.62313896856149142, 0.3932540034451326161 ) ) ;
#8130 = CARTESIAN_POINT ( 'NONE',  ( 9.116205194245099008, 21.95627871459122105, 1.667017424323884667 ) ) ;
#8131 = CARTESIAN_POINT ( 'NONE',  ( -47.86112874365709047, 43.41875999999999891, -23.29368419115692035 ) ) ;
#8132 = VERTEX_POINT ( 'NONE', #9961 ) ;
#8133 = VERTEX_POINT ( 'NONE', #3113 ) ;
#8134 = DIRECTION ( 'NONE',  ( 0.000000000000000000, 1.000000000000000000, 0.000000000000000000 ) ) ;
#8136 = LINE ( 'NONE', #6372, #6033 ) ;
#8135 = CARTESIAN_POINT ( 'NONE',  ( 4.297480147115120275, 20.54582653591270258, 0.4177457353544402618 ) ) ;
#8137 = ORIENTED_EDGE ( 'NONE', *, *, #5399, .T. ) ;
#8138 = CARTESIAN_POINT ( 'NONE',  ( 5.002037701870804653, 21.31635843410325037, 2.042759171744529478 ) ) ;
#8139 = EDGE_LOOP ( 'NONE', ( #11384, #10222, #3195, #15267, #17685, #4245, #12118, #14048, #16046, #8891, #20953, #16817 ) ) ;
#8140 = AXIS2_PLACEMENT_3D ( 'NONE', #1217, #21766, #18239 ) ;
#8141 = VERTEX_POINT ( 'NONE', #117 ) ;
#8142 = AXIS2_PLACEMENT_3D ( 'NONE', #8572, #18956, #1937 ) ;
#8143 = EDGE_CURVE ( 'NONE', #12037, #13767, #13625, .T. ) ;
#8144 = DIRECTION ( 'NONE',  ( 1.000000000000000000, 0.000000000000000000, 0.000000000000000000 ) ) ;
#8145 = EDGE_LOOP ( 'NONE', ( #17933, #3523, #20299, #4644 ) ) ;
#8146 = CARTESIAN_POINT ( 'NONE',  ( 2.211169688515047138, 12.61253923079801176, 2.196332706544586788 ) ) ;
#8147 = VECTOR ( 'NONE', #20688, 1000.000000000000000 ) ;
#8148 = CARTESIAN_POINT ( 'NONE',  ( 11.80762148770061337, 11.06331416201678053, -1.379479278252061958 ) ) ;
#8149 = EDGE_CURVE ( 'NONE', #15355, #7442, #6636, .T. ) ;
#8150 = EDGE_CURVE ( 'NONE', #13936, #2216, #21684, .T. ) ;
#8151 = LINE ( 'NONE', #11043, #3601 ) ;
#8152 = CARTESIAN_POINT ( 'NONE',  ( 12.88040283537677588, 39.28268749999999443, -0.09070320285213756550 ) ) ;
#8153 = AXIS2_PLACEMENT_3D ( 'NONE', #11985, #20932, #19162 ) ;
#8154 = DIRECTION ( 'NONE',  ( 0.000000000000000000, 1.000000000000000000, 0.000000000000000000 ) ) ;
#8155 = CARTESIAN_POINT ( 'NONE',  ( 1.807950215505384373, 13.11484105769346620, 0.4484171696861184442 ) ) ;
#8156 = CIRCLE ( 'NONE', #1107, 0.7950200000000000600 ) ;
#8157 = ORIENTED_EDGE ( 'NONE', *, *, #9944, .F. ) ;
#8158 = AXIS2_PLACEMENT_3D ( 'NONE', #18191, #11332, #11547 ) ;
#8159 = DIRECTION ( 'NONE',  ( 1.000000000000000000, 0.000000000000000000, 0.000000000000000000 ) ) ;
#8160 = CARTESIAN_POINT ( 'NONE',  ( 11.07961582054159244, 12.29391749999999739, -3.332761710603877159 ) ) ;
#8161 = DIRECTION ( 'NONE',  ( 0.000000000000000000, 1.000000000000000000, 0.000000000000000000 ) ) ;
#8162 = DIRECTION ( 'NONE',  ( 0.000000000000000000, -1.000000000000000000, 0.000000000000000000 ) ) ;
#8163 = ORIENTED_EDGE ( 'NONE', *, *, #6253, .T. ) ;
#8164 = ORIENTED_EDGE ( 'NONE', *, *, #13023, .F. ) ;
#8165 = CARTESIAN_POINT ( 'NONE',  ( 8.290641415794244296, 11.45164960235222118, 3.642276225269535317 ) ) ;
#8166 = CYLINDRICAL_SURFACE ( 'NONE', #12627, 1.984375000000000888 ) ;
#8167 = ORIENTED_EDGE ( 'NONE', *, *, #18725, .F. ) ;
#8168 = VECTOR ( 'NONE', #2898, 1000.000000000000000 ) ;
#8169 = ORIENTED_EDGE ( 'NONE', *, *, #17650, .T. ) ;
#8170 = DIRECTION ( 'NONE',  ( 0.000000000000000000, 1.000000000000000000, 0.000000000000000000 ) ) ;
#8171 = EDGE_CURVE ( 'NONE', #20855, #17145, #13516, .T. ) ;
#8172 = CARTESIAN_POINT ( 'NONE',  ( 8.011435824295395136, 11.80026701718135129, 1.025195225715891834 ) ) ;
#8173 = CIRCLE ( 'NONE', #8513, 30.16249999999999432 ) ;
#8174 = EDGE_CURVE ( 'NONE', #13027, #12952, #8956, .T. ) ;
#8175 = AXIS2_PLACEMENT_3D ( 'NONE', #4550, #18039, #3008 ) ;
#8176 = EDGE_CURVE ( 'NONE', #11803, #2298, #15974, .T. ) ;
#8177 = CIRCLE ( 'NONE', #9575, 0.5080000000000000071 ) ;
#8178 = CARTESIAN_POINT ( 'NONE',  ( 3.129583319975353550, 18.08847882444087674, 8.072846311850007339 ) ) ;
#8179 = CIRCLE ( 'NONE', #763, 30.16249999999999432 ) ;
#8180 = DIRECTION ( 'NONE',  ( -0.9964481331860212121, 0.000000000000000000, 0.08420877549337302259 ) ) ;
#8181 = DIRECTION ( 'NONE',  ( -0.9964481331860212121, 0.000000000000000000, 0.08420877549337300871 ) ) ;
#8182 = PLANE ( 'NONE',  #19566 ) ;
#8183 = CARTESIAN_POINT ( 'NONE',  ( 6.258027693244144984, 21.18174881316136293, 5.549184756157156784 ) ) ;
#8184 = CARTESIAN_POINT ( 'NONE',  ( -0.1855959611067334591, 15.75727966247650613, 0.07784262388770696317 ) ) ;
#8185 = CARTESIAN_POINT ( 'NONE',  ( 38.82016491058538321, 42.06303499999999929, -14.75770094105646812 ) ) ;
#8186 = ORIENTED_EDGE ( 'NONE', *, *, #4296, .F. ) ;
#8187 = CARTESIAN_POINT ( 'NONE',  ( 0.3055297026777472613, 20.17339616899437971, 6.156372013646721264 ) ) ;
#8188 = DIRECTION ( 'NONE',  ( 0.000000000000000000, 1.000000000000000000, 0.000000000000000000 ) ) ;
#8189 = CYLINDRICAL_SURFACE ( 'NONE', #18416, 1.190625000000000711 ) ;
#8190 = CARTESIAN_POINT ( 'NONE',  ( 18.48619651389723728, -7.612366584258952962, -14.31889584327733367 ) ) ;
#8191 = VECTOR ( 'NONE', #16880, 1000.000000000000000 ) ;
#8192 = VERTEX_POINT ( 'NONE', #18789 ) ;
#8193 = AXIS2_PLACEMENT_3D ( 'NONE', #4312, #655, #768 ) ;
#8194 = CARTESIAN_POINT ( 'NONE',  ( 9.385781312307386770, 16.63265789203856571, 8.122277095502592914 ) ) ;
#8195 = DIRECTION ( 'NONE',  ( -0.6702301885068632226, 0.000000000000000000, -0.7421532822901576454 ) ) ;
#8196 = CARTESIAN_POINT ( 'NONE',  ( 9.357963118639132105, 18.58272514913181084, -3.199465920211048697 ) ) ;
#8197 = ORIENTED_EDGE ( 'NONE', *, *, #7376, .T. ) ;
#8198 = AXIS2_PLACEMENT_3D ( 'NONE', #3957, #18758, #299 ) ;
#8199 = CARTESIAN_POINT ( 'NONE',  ( 6.370539475672911678, 20.77878503102673236, 0.03171506329460684059 ) ) ;
#8200 = VECTOR ( 'NONE', #1093, 1000.000000000000114 ) ;
#8201 = LINE ( 'NONE', #20011, #4918 ) ;
#8202 = CARTESIAN_POINT ( 'NONE',  ( -0.2885760015458498362, 20.30684170721071879, 4.831137852936522314 ) ) ;
#8203 = ADVANCED_FACE ( 'NONE', ( #13731 ), #15615, .T. ) ;
#8204 = LINE ( 'NONE', #11853, #14509 ) ;
#8205 = ADVANCED_FACE ( 'NONE', ( #13965 ), #10663, .T. ) ;
#8206 = CARTESIAN_POINT ( 'NONE',  ( 12.57635667311951622, 36.51313500000000545, 1.354834321244424267 ) ) ;
#8207 = ORIENTED_EDGE ( 'NONE', *, *, #15365, .T. ) ;
#8208 = AXIS2_PLACEMENT_3D ( 'NONE', #184, #21857, #11586 ) ;
#8209 = CARTESIAN_POINT ( 'NONE',  ( 9.655129386034436934, 13.52835235745250131, -2.703733241061648140 ) ) ;
#8210 = CARTESIAN_POINT ( 'NONE',  ( 4.950487383143544307, 20.46779201619338195, 6.708806423651408224 ) ) ;
#8211 = CARTESIAN_POINT ( 'NONE',  ( 20.76310168089343478, 36.51313500000000545, -11.26763008640078212 ) ) ;
#8212 = AXIS2_PLACEMENT_3D ( 'NONE', #7259, #278, #13787 ) ;
#8213 = AXIS2_PLACEMENT_3D ( 'NONE', #19302, #19196, #19406 ) ;
#8214 = CARTESIAN_POINT ( 'NONE',  ( 61.65536943582333151, 34.52875999999999834, -11.98363747855214712 ) ) ;
#8215 = CARTESIAN_POINT ( 'NONE',  ( 6.670151187356951894, 11.06004643669878185, 2.717775301413040800 ) ) ;
#8216 = CARTESIAN_POINT ( 'NONE',  ( 9.137394532338957376, -14.84248999999999974, -13.43583653331040750 ) ) ;
#8217 = DIRECTION ( 'NONE',  ( -0.9964481331860212121, 0.000000000000000000, 0.08420877549337302259 ) ) ;
#8218 = CARTESIAN_POINT ( 'NONE',  ( -23.01875000000000071, 0.000000000000000000, -3.968750000000000000 ) ) ;
#8219 = VERTEX_POINT ( 'NONE', #333 ) ;
#8220 = DIRECTION ( 'NONE',  ( 0.6744690509234938514, -0.7360996206939018904, -0.05699866455150646993 ) ) ;
#8221 = CARTESIAN_POINT ( 'NONE',  ( 32.42378190387104553, -1.983739999999999837, -18.15178106273469183 ) ) ;
#8222 = VECTOR ( 'NONE', #14086, 1000.000000000000000 ) ;
#8223 = ORIENTED_EDGE ( 'NONE', *, *, #3537, .F. ) ;
#8224 = CARTESIAN_POINT ( 'NONE',  ( 12.83070406023858823, 18.55124415177118991, 5.915695860297560671 ) ) ;
#8225 = LINE ( 'NONE', #20138, #4231 ) ;
#8226 = CARTESIAN_POINT ( 'NONE',  ( 17.45417163489883805, -7.133772557271947257, -14.59029241586745940 ) ) ;
#8227 = DIRECTION ( 'NONE',  ( 0.000000000000000000, 1.000000000000000000, 0.000000000000000000 ) ) ;
#8228 = EDGE_LOOP ( 'NONE', ( #17485, #3395, #3542, #10122 ) ) ;
#8229 =( LENGTH_UNIT ( ) NAMED_UNIT ( * ) SI_UNIT ( .MILLI., .METRE. ) );
#8230 = CARTESIAN_POINT ( 'NONE',  ( 0.02083138522552824973, 20.24316500000000119, 7.210477125664100484 ) ) ;
#8231 = CARTESIAN_POINT ( 'NONE',  ( 3.743459358786643598, 15.80679344681467846, -0.6324665095716647256 ) ) ;
#8232 = EDGE_CURVE ( 'NONE', #13313, #10898, #9588, .T. ) ;
#8233 = ORIENTED_EDGE ( 'NONE', *, *, #19106, .F. ) ;
#8234 = AXIS2_PLACEMENT_3D ( 'NONE', #10421, #8642, #1576 ) ;
#8235 = DIRECTION ( 'NONE',  ( 0.000000000000000000, -1.000000000000000000, -0.000000000000000000 ) ) ;
#8236 = CARTESIAN_POINT ( 'NONE',  ( 17.62224048108546626, -8.420204368612866475, -16.19806502325979025 ) ) ;
#8237 = VERTEX_POINT ( 'NONE', #10621 ) ;
#8238 = CARTESIAN_POINT ( 'NONE',  ( 5.952915771404345691, 18.80336625489407965, -0.8434118395857959083 ) ) ;
#8239 = CIRCLE ( 'NONE', #10007, 1.190624999999999378 ) ;
#8240 = LINE ( 'NONE', #1494, #12044 ) ;
#8241 = CARTESIAN_POINT ( 'NONE',  ( 11.45419627047315814, 15.66509967140728854, 7.663546619674057148 ) ) ;
#8242 = CARTESIAN_POINT ( 'NONE',  ( 14.02148737346195162, -6.731876932532799174, -16.48869785773486640 ) ) ;
#8243 = DIRECTION ( 'NONE',  ( -0.6702301885068628895, 0.000000000000000000, -0.7421532822901579785 ) ) ;
#8244 = AXIS2_PLACEMENT_3D ( 'NONE', #9402, #900, #13365 ) ;
#8245 = ORIENTED_EDGE ( 'NONE', *, *, #16838, .T. ) ;
#8246 = CARTESIAN_POINT ( 'NONE',  ( 9.574632210810730015, 21.03727855150343373, 2.997630161494908130 ) ) ;
#8247 = CARTESIAN_POINT ( 'NONE',  ( 9.173463358870977302, 17.37232422777100993, -3.665279000589813929 ) ) ;
#8248 = CARTESIAN_POINT ( 'NONE',  ( 29.64606458365116737, -1.985327499999998357, -15.53894806404596096 ) ) ;
#8249 = ORIENTED_EDGE ( 'NONE', *, *, #15671, .T. ) ;
#8250 = ORIENTED_EDGE ( 'NONE', *, *, #14460, .F. ) ;
#8251 = DIRECTION ( 'NONE',  ( 0.3542738219355867080, 0.000000000000000000, 0.9351417320872553729 ) ) ;
#8253 = CARTESIAN_POINT ( 'NONE',  ( 8.781357490942916399, -7.547927499999999235, -18.85455479843708559 ) ) ;
#8252 = CARTESIAN_POINT ( 'NONE',  ( 4.919162651895962135, 11.34514690749418087, 5.650005697289334883 ) ) ;
#8254 = ORIENTED_EDGE ( 'NONE', *, *, #9616, .F. ) ;
#8255 = CARTESIAN_POINT ( 'NONE',  ( 5.179964232832246829, 21.44866463646626187, 2.526011547878774799 ) ) ;
#8256 = CIRCLE ( 'NONE', #2257, 9.525000000000002132 ) ;
#8257 = ORIENTED_EDGE ( 'NONE', *, *, #12938, .T. ) ;
#8258 = ADVANCED_FACE ( 'NONE', ( #7079 ), #17252, .F. ) ;
#8259 = VERTEX_POINT ( 'NONE', #9059 ) ;
#8260 = DIRECTION ( 'NONE',  ( -0.9685006480810794960, 0.000000000000000000, -0.2490110332224836354 ) ) ;
#8261 = ORIENTED_EDGE ( 'NONE', *, *, #21034, .F. ) ;
#8262 = AXIS2_PLACEMENT_3D ( 'NONE', #9045, #15821, #17799 ) ;
#8263 = CARTESIAN_POINT ( 'NONE',  ( 12.91332895665777158, 20.46142704777525978, 5.469078331909021706 ) ) ;
#8264 = CARTESIAN_POINT ( 'NONE',  ( 46.03750000000000142, 32.54502000000000095, -10.31874999999999964 ) ) ;
#8265 = AXIS2_PLACEMENT_3D ( 'NONE', #21591, #19928, #4472 ) ;
#8266 = CARTESIAN_POINT ( 'NONE',  ( 56.91751438644678984, -1.983739999999999837, -20.96198986413465448 ) ) ;
#8267 = CARTESIAN_POINT ( 'NONE',  ( -15.41509608936259035, 37.15413452960619622, -10.31276839742836415 ) ) ;
#8268 = CARTESIAN_POINT ( 'NONE',  ( 1.933513631160261648, 18.30600127081370943, -0.3311359031021076094 ) ) ;
#8269 = ORIENTED_EDGE ( 'NONE', *, *, #19539, .T. ) ;
#8270 = DIRECTION ( 'NONE',  ( 0.000000000000000000, -1.000000000000000000, -0.000000000000000000 ) ) ;
#8271 = LINE ( 'NONE', #21757, #4329 ) ;
#8272 = CARTESIAN_POINT ( 'NONE',  ( 13.11001702788002277, 21.48322523121904482, 1.934949587800859572 ) ) ;
#8273 = EDGE_CURVE ( 'NONE', #13394, #14493, #5194, .T. ) ;
#8274 = CARTESIAN_POINT ( 'NONE',  ( 19.79362740382113728, -2.761185752867874932, -14.19488287356966971 ) ) ;
#8275 = EDGE_LOOP ( 'NONE', ( #19321, #20165, #20811, #18234, #1709 ) ) ;
#8276 = ORIENTED_EDGE ( 'NONE', *, *, #16436, .T. ) ;
#8277 = CARTESIAN_POINT ( 'NONE',  ( 11.02388696027891335, 18.13781435472470349, -3.406593805752508697 ) ) ;
#8278 = DIRECTION ( 'NONE',  ( 0.000000000000000000, 1.000000000000000000, -0.000000000000000000 ) ) ;
#8279 = VECTOR ( 'NONE', #3151, 1000.000000000000000 ) ;
#8280 = ORIENTED_EDGE ( 'NONE', *, *, #9225, .T. ) ;
#8281 = VERTEX_POINT ( 'NONE', #20550 ) ;
#8282 = DIRECTION ( 'NONE',  ( 1.000000000000000000, 0.000000000000000000, 0.000000000000000000 ) ) ;
#8283 = EDGE_CURVE ( 'NONE', #19832, #10623, #9941, .T. ) ;
#8284 = ORIENTED_EDGE ( 'NONE', *, *, #16836, .F. ) ;
#8285 = EDGE_CURVE ( 'NONE', #1068, #20066, #8177, .T. ) ;
#8286 = ADVANCED_FACE ( 'NONE', ( #5637 ), #20429, .F. ) ;
#8287 = CARTESIAN_POINT ( 'NONE',  ( 8.577308677684913008, 11.63761981776649179, 3.515469741029564776 ) ) ;
#8288 = CIRCLE ( 'NONE', #3355, 1.191259999999999319 ) ;
#8289 = CARTESIAN_POINT ( 'NONE',  ( 70.64340948846358970, 1.984375000000000000, -10.53785647675949910 ) ) ;
#8290 = DIRECTION ( 'NONE',  ( 0.000000000000000000, -1.000000000000000000, 0.000000000000000000 ) ) ;
#8291 = CARTESIAN_POINT ( 'NONE',  ( 0.3577463236909741440, 19.38239508688243617, 1.021447940004778454 ) ) ;
#8292 = LINE ( 'NONE', #15064, #14421 ) ;
#8293 = ORIENTED_EDGE ( 'NONE', *, *, #21610, .T. ) ;
#8294 = CARTESIAN_POINT ( 'NONE',  ( 2.246702380120268572, 13.47654819534348292, 0.8363802434591389723 ) ) ;
#8295 = DIRECTION ( 'NONE',  ( 0.000000000000000000, 1.000000000000000000, 0.000000000000000000 ) ) ;
#8296 = DIRECTION ( 'NONE',  ( 0.000000000000000000, 1.000000000000000000, 0.000000000000000000 ) ) ;
#8297 = LINE ( 'NONE', #16814, #5010 ) ;
#8298 = ADVANCED_FACE ( 'NONE', ( #12398 ), #15732, .F. ) ;
#8299 = AXIS2_PLACEMENT_3D ( 'NONE', #9592, #16361, #21420 ) ;
#8300 = EDGE_LOOP ( 'NONE', ( #10554, #20666, #4501, #4410 ) ) ;
#8301 = CARTESIAN_POINT ( 'NONE',  ( 8.701198850936064488, 20.20358612698620249, 6.625331775719724092 ) ) ;
#8302 = CARTESIAN_POINT ( 'NONE',  ( 49.81956284419040060, 30.56064500000000095, 11.98436472153758103 ) ) ;
#8303 = CARTESIAN_POINT ( 'NONE',  ( 9.670731391893321316, 19.91002294283195795, -2.452946502561233810 ) ) ;
#8304 = VERTEX_POINT ( 'NONE', #11947 ) ;
#8305 = CARTESIAN_POINT ( 'NONE',  ( 6.593580017284943473, 21.14855486304147192, 0.6275595558785633798 ) ) ;
#8306 = CARTESIAN_POINT ( 'NONE',  ( 32.96560389001691505, 34.52875999999999834, -17.84002872454335886 ) ) ;
#8307 = DIRECTION ( 'NONE',  ( -0.6702301885068634446, 0.000000000000000000, -0.7421532822901576454 ) ) ;
#8308 = EDGE_CURVE ( 'NONE', #6054, #4933, #14068, .T. ) ;
#8309 = CARTESIAN_POINT ( 'NONE',  ( 55.52866846859686234, 34.52875999999999834, -11.12083858657437752 ) ) ;
#8310 = CARTESIAN_POINT ( 'NONE',  ( 7.038768548784214651, 18.13751136180625778, 7.270069188298340812 ) ) ;
#8311 = CARTESIAN_POINT ( 'NONE',  ( 2.063749999518360134, 30.56070453124999986, 10.71562494997783865 ) ) ;
#8312 = CIRCLE ( 'NONE', #17144, 0.5080000000000013394 ) ;
#8313 = CARTESIAN_POINT ( 'NONE',  ( -2.607150795738780058, 32.54502000000000095, 8.731885000000000119 ) ) ;
#8314 = CARTESIAN_POINT ( 'NONE',  ( 7.290540035995150880, 11.65642365002708125, 4.787114039832606416 ) ) ;
#8315 = CARTESIAN_POINT ( 'NONE',  ( -15.40791870508676631, -4.601685412415895904, -10.30897195950450573 ) ) ;
#8316 = CARTESIAN_POINT ( 'NONE',  ( 1.382092486215193761, 18.94469375348566231, 8.962251623514621457 ) ) ;
#8317 = DIRECTION ( 'NONE',  ( 0.000000000000000000, 1.000000000000000000, 0.000000000000000000 ) ) ;
#8318 = DIRECTION ( 'NONE',  ( 0.9943660382494290406, 0.000000000000000000, -0.1060008583745199739 ) ) ;
#8319 = CARTESIAN_POINT ( 'NONE',  ( 1.833072101810493848, 14.88386107855003360, 0.2418471280350485975 ) ) ;
#8320 = CARTESIAN_POINT ( 'NONE',  ( 7.735533989518945219, 5.548947500000001476, -21.17236077523805449 ) ) ;
#8321 = CARTESIAN_POINT ( 'NONE',  ( 13.55088323884965718, -7.823075611188723855, -16.61323137860442856 ) ) ;
#8322 = EDGE_CURVE ( 'NONE', #12596, #10374, #8729, .T. ) ;
#8323 = EDGE_CURVE ( 'NONE', #1499, #3169, #3545, .T. ) ;
#8324 = CARTESIAN_POINT ( 'NONE',  ( 23.49608546833631451, 28.96330250000000461, -17.12016812500874252 ) ) ;
#8325 = EDGE_CURVE ( 'NONE', #1509, #5503, #4303, .T. ) ;
#8326 = VERTEX_POINT ( 'NONE', #225 ) ;
#8327 = DIRECTION ( 'NONE',  ( 0.9579671649362033747, 0.000000000000000000, -0.2868778675745011775 ) ) ;
#8328 = CARTESIAN_POINT ( 'NONE',  ( 10.83572638560662327, 12.10937221960885246, 4.528287571500745123 ) ) ;
#8329 = CARTESIAN_POINT ( 'NONE',  ( -29.36874999999999858, 1.984375000000000000, 8.731249999999999289 ) ) ;
#8330 = CARTESIAN_POINT ( 'NONE',  ( 12.66561601154539041, 19.21253279861005581, 5.535559188462356062 ) ) ;
#8331 = CARTESIAN_POINT ( 'NONE',  ( 28.38195592936287781, 30.55334249999999940, -13.81504834214261024 ) ) ;
#8332 = CARTESIAN_POINT ( 'NONE',  ( 6.269352038965187113, 10.97123987517479016, 2.325299610618768220 ) ) ;
#8333 = CARTESIAN_POINT ( 'NONE',  ( 11.38821987747605391, -3.675948036407177710, -15.27230885423398199 ) ) ;
#8335 = LINE ( 'NONE', #14780, #21576 ) ;
#8334 = CARTESIAN_POINT ( 'NONE',  ( 1.385961804465817515, 14.30904236277701003, 8.449454185675360662 ) ) ;
#8336 = ORIENTED_EDGE ( 'NONE', *, *, #8842, .T. ) ;
#8337 = CARTESIAN_POINT ( 'NONE',  ( -0.1849527131266449076, 20.23672349358593792, 5.150944217628095068 ) ) ;
#8338 = DIRECTION ( 'NONE',  ( -0.2868778675745010664, 0.000000000000000000, -0.9579671649362032637 ) ) ;
#8339 = LINE ( 'NONE', #13440, #20986 ) ;
#8340 = ORIENTED_EDGE ( 'NONE', *, *, #16884, .F. ) ;
#8341 = CARTESIAN_POINT ( 'NONE',  ( 13.17838052650600211, 14.87494513186989664, 6.319450451114021483 ) ) ;
#8342 = CARTESIAN_POINT ( 'NONE',  ( 12.44399840006683178, 11.21920808676120274, 2.553881509949003092 ) ) ;
#8343 = LINE ( 'NONE', #18297, #13126 ) ;
#8344 = CARTESIAN_POINT ( 'NONE',  ( 11.10986520838597613, 18.39193805972391971, -4.138733212223557167 ) ) ;
#8345 = CARTESIAN_POINT ( 'NONE',  ( 16.95801165930927823, -7.124051013253036579, -15.87873232967992543 ) ) ;
#8346 = EDGE_CURVE ( 'NONE', #9048, #21748, #5956, .T. ) ;
#8347 = LINE ( 'NONE', #18405, #16172 ) ;
#8348 = VECTOR ( 'NONE', #10940, 1000.000000000000114 ) ;
#8349 = VERTEX_POINT ( 'NONE', #12844 ) ;
#8350 = CARTESIAN_POINT ( 'NONE',  ( 8.168579537737969076, 19.82474022107643208, -0.7181693113545990492 ) ) ;
#8351 = CARTESIAN_POINT ( 'NONE',  ( 5.801569891678039603, 19.23834655595790011, -1.510785752356017975 ) ) ;
#8352 = DIRECTION ( 'NONE',  ( 0.9685006480810790519, 0.000000000000000000, 0.2490110332224857170 ) ) ;
#8353 = ORIENTED_EDGE ( 'NONE', *, *, #10185, .F. ) ;
#8354 = ORIENTED_EDGE ( 'NONE', *, *, #16026, .T. ) ;
#8355 = DIRECTION ( 'NONE',  ( -0.2490110332224836354, 0.000000000000000000, 0.9685006480810794960 ) ) ;
#8356 = CARTESIAN_POINT ( 'NONE',  ( -0.04771496096788591101, 12.52330284320706077, 1.689320059643299565 ) ) ;
#8357 = ORIENTED_EDGE ( 'NONE', *, *, #11423, .T. ) ;
#8358 = CARTESIAN_POINT ( 'NONE',  ( 6.874689736735521528, 19.87943235501797545, 7.077769955840262028 ) ) ;
#8359 = ORIENTED_EDGE ( 'NONE', *, *, #20820, .T. ) ;
#8360 = VECTOR ( 'NONE', #14033, 1000.000000000000000 ) ;
#8361 = LINE ( 'NONE', #3176, #2233 ) ;
#8362 = ORIENTED_EDGE ( 'NONE', *, *, #10292, .T. ) ;
#8363 = B_SPLINE_CURVE_WITH_KNOTS ( 'NONE', 3,
 ( #15995, #2593, #7570, #929, #14331, #12660, #21151, #19386, #12776, #19499, #4362, #3032 ),
 .UNSPECIFIED., .F., .F.,
 ( 4, 2, 2, 2, 2, 4 ),
 ( 0.001233369978144762671, 0.001719813969628884937, 0.001963035965370948238, 0.002206257961113011756, 0.002692701952597139660, 0.003179145944081267997 ),
 .UNSPECIFIED. ) ;
#8364 = CARTESIAN_POINT ( 'NONE',  ( 66.03921914090641110, 30.56064500000000095, -10.93409647675949969 ) ) ;
#8365 = CARTESIAN_POINT ( 'NONE',  ( 39.18468883297455818, 40.07906110073898276, -4.105455453847051572 ) ) ;
#8366 = CARTESIAN_POINT ( 'NONE',  ( 2.303762633758687173, 19.73751257430979678, 0.5328489609499682533 ) ) ;
#8367 = EDGE_CURVE ( 'NONE', #16212, #777, #12722, .T. ) ;
#8368 = ORIENTED_EDGE ( 'NONE', *, *, #20284, .T. ) ;
#8369 = CYLINDRICAL_SURFACE ( 'NONE', #1861, 0.7950200000000003930 ) ;
#8370 = DIRECTION ( 'NONE',  ( -0.000000000000000000, -1.000000000000000000, 0.000000000000000000 ) ) ;
#8371 = CARTESIAN_POINT ( 'NONE',  ( 29.15193331460030279, 30.55334249999999940, -13.61707959051006966 ) ) ;
#8372 = DIRECTION ( 'NONE',  ( -0.9966381950048638361, 0.000000000000000000, 0.08192867786951606168 ) ) ;
#8373 = VERTEX_POINT ( 'NONE', #11269 ) ;
#8374 = ORIENTED_EDGE ( 'NONE', *, *, #17598, .T. ) ;
#8375 = CARTESIAN_POINT ( 'NONE',  ( 10.98303339775889498, 12.79277479448814248, -2.359408852867018958 ) ) ;
#8376 = VECTOR ( 'NONE', #5926, 1000.000000000000227 ) ;
#8377 = VERTEX_POINT ( 'NONE', #9496 ) ;
#8378 = ORIENTED_EDGE ( 'NONE', *, *, #6781, .F. ) ;
#8379 = DIRECTION ( 'NONE',  ( 1.000000000000000000, 0.000000000000000000, 0.000000000000000000 ) ) ;
#8380 = ORIENTED_EDGE ( 'NONE', *, *, #3975, .T. ) ;
#8381 = CARTESIAN_POINT ( 'NONE',  ( 9.190889634080209092, 16.82461965218397282, 7.202071835226256269 ) ) ;
#8382 = CARTESIAN_POINT ( 'NONE',  ( -22.30848347979677371, -1.587500000000002132, 1.064728033956552578 ) ) ;
#8383 = FACE_OUTER_BOUND ( 'NONE', #3262, .T. ) ;
#8384 = VECTOR ( 'NONE', #16165, 1000.000000000000000 ) ;
#8385 = CARTESIAN_POINT ( 'NONE',  ( -1.427050033073577806, 5.548947500000001476, -23.44038945102687066 ) ) ;
#8386 = DIRECTION ( 'NONE',  ( -0.2490110332224849676, 0.000000000000000000, 0.9685006480810792739 ) ) ;
#8387 = CARTESIAN_POINT ( 'NONE',  ( 0.1737502244468468182, 12.20094924675537307, 2.251015528918583808 ) ) ;
#8388 = ADVANCED_FACE ( 'NONE', ( #19565, #20887 ), #4204, .T. ) ;
#8389 = DIRECTION ( 'NONE',  ( 0.08420877549337300871, 0.000000000000000000, 0.9964481331860212121 ) ) ;
#8390 = EDGE_CURVE ( 'NONE', #16118, #12232, #775, .T. ) ;
#8391 = ORIENTED_EDGE ( 'NONE', *, *, #20331, .F. ) ;
#8392 = CARTESIAN_POINT ( 'NONE',  ( 1.061577872868078254, 12.03899270364792073, 4.769622043989930837 ) ) ;
#8393 = PLANE ( 'NONE',  #11013 ) ;
#8394 = CARTESIAN_POINT ( 'NONE',  ( 53.00094895929537842, -7.547610000000004149, -16.81958146583652791 ) ) ;
#8395 = LINE ( 'NONE', #13302, #20900 ) ;
#8396 = ORIENTED_EDGE ( 'NONE', *, *, #10058, .F. ) ;
#8397 = CARTESIAN_POINT ( 'NONE',  ( 10.63989556519935320, 19.52774875955264022, 6.752680363256145846 ) ) ;
#8398 = CARTESIAN_POINT ( 'NONE',  ( 10.62635245719450694, 21.77196383837482330, 0.09988737663030886060 ) ) ;
#8399 = VERTEX_POINT ( 'NONE', #9280 ) ;
#8400 = VECTOR ( 'NONE', #12621, 1000.000000000000000 ) ;
#8401 = CARTESIAN_POINT ( 'NONE',  ( 8.557020710820847142, 10.80609942023040126, 3.389879254953236831 ) ) ;
#8402 = CARTESIAN_POINT ( 'NONE',  ( 3.386193242415981075, 13.61441523003558274, 7.601052676155180876 ) ) ;
#8403 = LINE ( 'NONE', #3553, #15844 ) ;
#8404 =( GEOMETRIC_REPRESENTATION_CONTEXT ( 3 ) GLOBAL_UNCERTAINTY_ASSIGNED_CONTEXT ( ( #15883 ) ) GLOBAL_UNIT_ASSIGNED_CONTEXT ( ( #17409, #18713, #14103 ) ) REPRESENTATION_CONTEXT ( 'NONE', 'WORKASPACE' ) );
#8405 = CARTESIAN_POINT ( 'NONE',  ( 21.24465364422600189, 16.26393749999999727, -2.595505584112000275 ) ) ;
#8406 = EDGE_CURVE ( 'NONE', #4430, #18428, #11720, .T. ) ;
#8407 = CARTESIAN_POINT ( 'NONE',  ( 10.78492640469823982, 20.67808185030680335, 5.014337372028484729 ) ) ;
#8408 = CARTESIAN_POINT ( 'NONE',  ( 34.72145145287101542, -1.983739999999999837, 0.5851394578805096947 ) ) ;
#8409 = CARTESIAN_POINT ( 'NONE',  ( -0.1089046874588744940, 17.37668286801814688, 0.03726443620168150284 ) ) ;
#8410 = DIRECTION ( 'NONE',  ( -0.9987059298363657467, 0.000000000000000000, -0.05085730733808445370 ) ) ;
#8411 = VECTOR ( 'NONE', #6675, 1000.000000000000000 ) ;
#8412 = EDGE_CURVE ( 'NONE', #18743, #11237, #16055, .T. ) ;
#8413 = CARTESIAN_POINT ( 'NONE',  ( 20.10279225084434174, -0.7360295338183041602, -14.79594426830372278 ) ) ;
#8414 = CARTESIAN_POINT ( 'NONE',  ( 1.471179364221197883, 15.70105570582070520, 8.896772800854545693 ) ) ;
#8415 = CARTESIAN_POINT ( 'NONE',  ( 53.28913209022548614, -6.356984999999999886, -15.26333197569509714 ) ) ;
#8416 = CARTESIAN_POINT ( 'NONE',  ( 12.88040283537677588, 12.29391749999999739, -0.09070320285213756550 ) ) ;
#8417 = CARTESIAN_POINT ( 'NONE',  ( 10.88228110427572659, -4.361565139864056029, -17.13396526837493994 ) ) ;
#8418 = FACE_OUTER_BOUND ( 'NONE', #20714, .T. ) ;
#8419 = ORIENTED_EDGE ( 'NONE', *, *, #14543, .T. ) ;
#8420 = FACE_BOUND ( 'NONE', #20924, .T. ) ;
#8421 = CARTESIAN_POINT ( 'NONE',  ( 9.285792827353402501, 21.87697856516881956, 2.219697743754897257 ) ) ;
#8422 = DIRECTION ( 'NONE',  ( 0.7421532822901579785, 0.000000000000000000, -0.6702301885068630005 ) ) ;
#8423 = DIRECTION ( 'NONE',  ( -0.000000000000000000, -1.000000000000000000, 0.000000000000000000 ) ) ;
#8424 = CARTESIAN_POINT ( 'NONE',  ( 13.11122246924493417, 16.59952282105541954, 6.404990385722812540 ) ) ;
#8425 = CARTESIAN_POINT ( 'NONE',  ( 12.02474915109715603, -1.983739999999999393, -13.51434638588835391 ) ) ;
#8426 = CARTESIAN_POINT ( 'NONE',  ( 19.07381010491119255, -0.2526079255638566390, -14.35716343207643675 ) ) ;
#8427 = CARTESIAN_POINT ( 'NONE',  ( 3.081105562148156007, 13.56078169262926281, 7.763509864629036805 ) ) ;
#8428 = ORIENTED_EDGE ( 'NONE', *, *, #9889, .F. ) ;
#8429 = DIRECTION ( 'NONE',  ( 0.000000000000000000, 0.000000000000000000, 1.000000000000000000 ) ) ;
#8430 = DIRECTION ( 'NONE',  ( -0.6702301885068630005, 0.000000000000000000, -0.7421532822901579785 ) ) ;
#8431 = CARTESIAN_POINT ( 'NONE',  ( 3.831872794198578180, 16.97575148034115244, -0.6279392605359102042 ) ) ;
#8432 = CARTESIAN_POINT ( 'NONE',  ( 65.90927232300019512, 1.984375000000000000, -13.30734117861468135 ) ) ;
#8433 = AXIS2_PLACEMENT_3D ( 'NONE', #16890, #7045, #17332 ) ;
#8434 = CARTESIAN_POINT ( 'NONE',  ( 6.253898308320673394, 11.68813189510091100, 2.888293778337470918 ) ) ;
#8435 = ADVANCED_FACE ( 'NONE', ( #21007 ), #7736, .T. ) ;
#8436 = EDGE_CURVE ( 'NONE', #3189, #180, #756, .T. ) ;
#8437 = CIRCLE ( 'NONE', #3916, 0.7950200000000000600 ) ;
#8438 = EDGE_CURVE ( 'NONE', #13139, #18598, #13141, .T. ) ;
#8439 = VERTEX_POINT ( 'NONE', #21105 ) ;
#8440 = CARTESIAN_POINT ( 'NONE',  ( 6.927322632701765848, 20.81446147317312168, 1.621339958521637703 ) ) ;
#8441 = CARTESIAN_POINT ( 'NONE',  ( 4.054711315827309370, 20.40797957536717178, 5.161551740127496402 ) ) ;
#8442 = AXIS2_PLACEMENT_3D ( 'NONE', #9529, #9197, #5885 ) ;
#8443 = CARTESIAN_POINT ( 'NONE',  ( 9.392652412154310682, 17.21976690206051330, -2.901007874484461624 ) ) ;
#8444 = CARTESIAN_POINT ( 'NONE',  ( 4.464807677231505068, 20.92444076583792167, 5.032481929441805057 ) ) ;
#8445 = CARTESIAN_POINT ( 'NONE',  ( 9.062801421126779999, 21.95627871459122105, 1.683009998091938852 ) ) ;
#8446 = CARTESIAN_POINT ( 'NONE',  ( 17.31838635957196715, -7.011879312349825533, -15.80413428893090355 ) ) ;
#8447 = CARTESIAN_POINT ( 'NONE',  ( 10.68528288545773641, -4.809670885807078022, -15.81083395943519854 ) ) ;
#8448 = ORIENTED_EDGE ( 'NONE', *, *, #5349, .F. ) ;
#8449 = CARTESIAN_POINT ( 'NONE',  ( 10.80473891853958612, 18.82471788637430166, 6.156953377096570534 ) ) ;
#8450 = CARTESIAN_POINT ( 'NONE',  ( 11.15456943723388861, 18.39169315105245417, -4.151439798146012272 ) ) ;
#8451 = CARTESIAN_POINT ( 'NONE',  ( 35.15748561355322011, 34.52875999999999834, 0.3244898641346534163 ) ) ;
#8452 = VERTEX_POINT ( 'NONE', #9390 ) ;
#8453 = VERTEX_POINT ( 'NONE', #6187 ) ;
#8454 = CARTESIAN_POINT ( 'NONE',  ( -18.18961309330695997, -3.266559801243759331, -25.80119252674831998 ) ) ;
#8455 = CARTESIAN_POINT ( 'NONE',  ( 10.93940955106799073, 14.41445727887342620, -4.025580141893404296 ) ) ;
#8456 = AXIS2_PLACEMENT_3D ( 'NONE', #19828, #16635, #6463 ) ;
#8458 = DIRECTION ( 'NONE',  ( 0.5087559856598092844, 0.000000000000000000, 0.8609107660235849613 ) ) ;
#8457 = CARTESIAN_POINT ( 'NONE',  ( 3.513474866157187293, 12.26666322754141980, 0.5275322538260243110 ) ) ;
#8459 = ORIENTED_EDGE ( 'NONE', *, *, #8673, .F. ) ;
#8460 = CARTESIAN_POINT ( 'NONE',  ( 5.008754897235177417, 21.32213879784493926, 2.060963987967154853 ) ) ;
#8461 = AXIS2_PLACEMENT_3D ( 'NONE', #14083, #20910, #2340 ) ;
#8462 = VERTEX_POINT ( 'NONE', #16158 ) ;
#8463 = ADVANCED_FACE ( 'NONE', ( #14497 ), #12955, .T. ) ;
#8464 = AXIS2_PLACEMENT_3D ( 'NONE', #20014, #5204, #13524 ) ;
#8465 = LINE ( 'NONE', #21852, #9696 ) ;
#8466 = EDGE_LOOP ( 'NONE', ( #18648, #9569, #2189 ) ) ;
#8467 = APPLICATION_CONTEXT ( 'automotive_design' ) ;
#8468 = CARTESIAN_POINT ( 'NONE',  ( 3.808323415348045415, 13.81725641533127202, 0.1165697555046887185 ) ) ;
#8469 = AXIS2_PLACEMENT_3D ( 'NONE', #9078, #17718, #15853 ) ;
#8470 = CARTESIAN_POINT ( 'NONE',  ( 14.05820270259704152, 36.51313500000000545, -15.03781736451272444 ) ) ;
#8471 = CARTESIAN_POINT ( 'NONE',  ( 39.58386072796507449, 40.07865999999999929, -4.490541772578644064 ) ) ;
#8472 = CYLINDRICAL_SURFACE ( 'NONE', #21021, 0.5079999999999984528 ) ;
#8473 = CARTESIAN_POINT ( 'NONE',  ( 2.850083250245388111, 20.85896612695718133, 1.947395870406601226 ) ) ;
#8474 = ORIENTED_EDGE ( 'NONE', *, *, #2395, .F. ) ;
#8475 = CARTESIAN_POINT ( 'NONE',  ( 59.65121809612895731, 34.52875999999999834, -2.485718937265306572 ) ) ;
#8476 = DIRECTION ( 'NONE',  ( -1.000000000000000000, 0.000000000000000000, 0.000000000000000000 ) ) ;
#8477 = SURFACE_SIDE_STYLE ('',( #2060 ) ) ;
#8478 = CARTESIAN_POINT ( 'NONE',  ( 9.335363283976800375, 34.52875999999999834, -14.20581391854862474 ) ) ;
#8480 = CARTESIAN_POINT ( 'NONE',  ( 15.24277482227980407, -7.221304072066160096, -15.02133152971018326 ) ) ;
#8479 = CARTESIAN_POINT ( 'NONE',  ( 59.65121809612895731, 32.54502000000000095, -2.485718937265306572 ) ) ;
#8481 = VERTEX_POINT ( 'NONE', #12614 ) ;
#8482 = ORIENTED_EDGE ( 'NONE', *, *, #3741, .F. ) ;
#8483 = CARTESIAN_POINT ( 'NONE',  ( 7.563702072044085511, 18.07137575567074350, -1.907521650424996107 ) ) ;
#8484 = CIRCLE ( 'NONE', #20838, 3.970020000000002991 ) ;
#8486 = DIRECTION ( 'NONE',  ( 0.000000000000000000, 1.000000000000000000, 0.000000000000000000 ) ) ;
#8485 = CARTESIAN_POINT ( 'NONE',  ( 0.7026925879561919386, 20.32382785537196312, 1.796361731335691436 ) ) ;
#8487 = ORIENTED_EDGE ( 'NONE', *, *, #7490, .T. ) ;
#8488 = ORIENTED_EDGE ( 'NONE', *, *, #5082, .T. ) ;
#8489 = DIRECTION ( 'NONE',  ( 1.000000000000000000, 0.000000000000000000, 0.000000000000000000 ) ) ;
#8490 = ORIENTED_EDGE ( 'NONE', *, *, #11017, .T. ) ;
#8491 = CARTESIAN_POINT ( 'NONE',  ( 8.556392325919617292, 11.61851416689291305, 3.423200530932141383 ) ) ;
#8492 = DIRECTION ( 'NONE',  ( 0.2145948757085688052, 0.000000000000000000, 0.9767031480033347979 ) ) ;
#8493 = EDGE_CURVE ( 'NONE', #7268, #10232, #19337, .T. ) ;
#8494 = CIRCLE ( 'NONE', #16643, 2.381250000000001421 ) ;
#8495 = AXIS2_PLACEMENT_3D ( 'NONE', #21187, #9364, #12695 ) ;
#8496 = DIRECTION ( 'NONE',  ( -0.000000000000000000, -1.000000000000000000, 0.000000000000000000 ) ) ;
#8497 = DIRECTION ( 'NONE',  ( 0.000000000000000000, -1.000000000000000000, 0.000000000000000000 ) ) ;
#8498 = CARTESIAN_POINT ( 'NONE',  ( -0.1352155204582886072, 16.66627892838214464, 0.04119029793672387973 ) ) ;
#8499 = LINE ( 'NONE', #10394, #11211 ) ;
#8500 = ADVANCED_FACE ( 'NONE', ( #15947 ), #7955, .T. ) ;
#8501 = ORIENTED_EDGE ( 'NONE', *, *, #8938, .T. ) ;
#8502 = CARTESIAN_POINT ( 'NONE',  ( 4.328347590241748755, 12.03379079558084186, 2.230145814812864113 ) ) ;
#8503 = DIRECTION ( 'NONE',  ( -0.000000000000000000, -1.000000000000000000, 0.000000000000000000 ) ) ;
#8504 = DIRECTION ( 'NONE',  ( -0.6702301885068632226, 0.000000000000000000, -0.7421532822901576454 ) ) ;
#8505 = DIRECTION ( 'NONE',  ( -0.06191955310929833645, 0.000000000000000000, 0.9980811434661738257 ) ) ;
#8506 = AXIS2_PLACEMENT_3D ( 'NONE', #3906, #7431, #5781 ) ;
#8507 = CARTESIAN_POINT ( 'NONE',  ( 21.25660046192028929, 34.52875999999999834, -13.18703856829094079 ) ) ;
#8508 = ORIENTED_EDGE ( 'NONE', *, *, #16336, .T. ) ;
#8509 = CARTESIAN_POINT ( 'NONE',  ( 12.94563250920762520, 12.79228088949424169, 6.166948107170512117 ) ) ;
#8510 = CARTESIAN_POINT ( 'NONE',  ( 39.42154620619601957, -6.356984999999999886, -4.343957374021048423 ) ) ;
#8511 = CARTESIAN_POINT ( 'NONE',  ( 13.33056277106260978, 16.75682411354094015, 7.157340733298330981 ) ) ;
#8512 = ORIENTED_EDGE ( 'NONE', *, *, #15233, .T. ) ;
#8513 = AXIS2_PLACEMENT_3D ( 'NONE', #17170, #15653, #20925 ) ;
#8514 = ORIENTED_EDGE ( 'NONE', *, *, #21801, .T. ) ;
#8515 = VECTOR ( 'NONE', #11059, 1000.000000000000000 ) ;
#8516 = CARTESIAN_POINT ( 'NONE',  ( 9.107277861881895475, 11.81316815476289506, 5.756061362039455176 ) ) ;
#8517 = CARTESIAN_POINT ( 'NONE',  ( 3.474038444628396949, 20.64378046205170136, 3.586838031231339485 ) ) ;
#8518 = CARTESIAN_POINT ( 'NONE',  ( 14.93145837000203358, 15.36419388438619826, -20.01065317369261365 ) ) ;
#8519 = CARTESIAN_POINT ( 'NONE',  ( 31.06384331886062711, 2.019535839764540430, 1.146004012482531476 ) ) ;
#8520 = EDGE_CURVE ( 'NONE', #14184, #8937, #6056, .T. ) ;
#8521 = DIRECTION ( 'NONE',  ( 0.000000000000000000, -1.000000000000000000, 0.000000000000000000 ) ) ;
#8522 = LINE ( 'NONE', #3673, #11280 ) ;
#8523 = CARTESIAN_POINT ( 'NONE',  ( 12.97329811073338846, 20.23326750546686270, 5.220295724011733363 ) ) ;
#8524 = CARTESIAN_POINT ( 'NONE',  ( 6.364250290165353263, 10.85153064243760213, 2.321502149683346783 ) ) ;
#8525 = DIRECTION ( 'NONE',  ( 0.000000000000000000, 0.000000000000000000, -1.000000000000000000 ) ) ;
#8526 = AXIS2_PLACEMENT_3D ( 'NONE', #2683, #15755, #14311 ) ;
#8527 = VECTOR ( 'NONE', #15265, 1000.000000000000000 ) ;
#8528 = CARTESIAN_POINT ( 'NONE',  ( 20.19045750888530577, -1.020013971529757368, -14.77085460577932885 ) ) ;
#8529 = CARTESIAN_POINT ( 'NONE',  ( 5.176227073658261624, 12.95116610613770369, 6.671170083817433927 ) ) ;
#8530 = FACE_OUTER_BOUND ( 'NONE', #14003, .T. ) ;
#8531 = CARTESIAN_POINT ( 'NONE',  ( 11.42902352243642028, -5.736415193692209868, -17.04764026735380611 ) ) ;
#8532 = ORIENTED_EDGE ( 'NONE', *, *, #16140, .T. ) ;
#8533 = LINE ( 'NONE', #10196, #11395 ) ;
#8534 = CIRCLE ( 'NONE', #14575, 3.174999999999998490 ) ;
#8535 = CARTESIAN_POINT ( 'NONE',  ( 10.96673932127253970, 12.57086297534474717, 5.140911593025348836 ) ) ;
#8536 = CARTESIAN_POINT ( 'NONE',  ( 10.89554121559266164, 19.63180904864239196, 6.552446325582041986 ) ) ;
#8537 = EDGE_CURVE ( 'NONE', #21183, #16767, #2175, .T. ) ;
#8538 = CARTESIAN_POINT ( 'NONE',  ( 17.02725982432203367, 128.5105379999999968, -14.27444360421403857 ) ) ;
#8539 = ORIENTED_EDGE ( 'NONE', *, *, #9567, .F. ) ;
#8540 = CARTESIAN_POINT ( 'NONE',  ( 12.42688504315472287, 11.33449225177425213, 2.569421434122930670 ) ) ;
#8541 = LINE ( 'NONE', #5442, #17618 ) ;
#8543 = CARTESIAN_POINT ( 'NONE',  ( 32.42378190387104553, 0.000000000000000000, -18.15178106273469183 ) ) ;
#8542 = CARTESIAN_POINT ( 'NONE',  ( 6.404761471570224352, 19.58301787754098200, 6.631544299425215172 ) ) ;
#8544 = ORIENTED_EDGE ( 'NONE', *, *, #7769, .T. ) ;
#8545 = APPLICATION_PROTOCOL_DEFINITION ( 'draft international standard', 'automotive_design', 1998, #20907 ) ;
#8546 = DIRECTION ( 'NONE',  ( -0.08420877549337300871, 0.000000000000000000, -0.9964481331860212121 ) ) ;
#8547 = VECTOR ( 'NONE', #12353, 1000.000000000000000 ) ;
#8548 = DIRECTION ( 'NONE',  ( 0.000000000000000000, 1.000000000000000000, 0.000000000000000000 ) ) ;
#8549 = EDGE_CURVE ( 'NONE', #21755, #17754, #19236, .T. ) ;
#8550 = EDGE_CURVE ( 'NONE', #7171, #18389, #5720, .T. ) ;
#8551 = EDGE_CURVE ( 'NONE', #6728, #3226, #1826, .T. ) ;
#8552 = CARTESIAN_POINT ( 'NONE',  ( 6.124889344102976807, 11.59927643492120097, 2.920436077416646903 ) ) ;
#8553 = VERTEX_POINT ( 'NONE', #3855 ) ;
#8554 = VECTOR ( 'NONE', #9127, 1000.000000000000114 ) ;
#8555 = CARTESIAN_POINT ( 'NONE',  ( 7.544623071831273897, 13.14813038638666143, -1.051744186015200588 ) ) ;
#8556 = CARTESIAN_POINT ( 'NONE',  ( 11.74386382974287812, 19.71606648096064163, -2.545816756848700013 ) ) ;
#8557 = CARTESIAN_POINT ( 'NONE',  ( 5.006421629233452464, 11.37607716600946084, 3.684801207120545374 ) ) ;
#8558 = CARTESIAN_POINT ( 'NONE',  ( 9.198481203478936052, 18.56541443352003640, 7.659581353093840583 ) ) ;
#8559 = CARTESIAN_POINT ( 'NONE',  ( 11.89249479014546473, -3.409559102863189750, -16.84257439245622834 ) ) ;
#8560 = UNCERTAINTY_MEASURE_WITH_UNIT (LENGTH_MEASURE( 1.000000000000000082E-05 ), #19486, 'distance_accuracy_value', 'NONE');
#8561 = LINE ( 'NONE', #3384, #13441 ) ;
#8562 = ORIENTED_EDGE ( 'NONE', *, *, #272, .T. ) ;
#8563 = CARTESIAN_POINT ( 'NONE',  ( 11.03326096593770167, 17.69443056144524107, 6.636539859302792443 ) ) ;
#8564 = CARTESIAN_POINT ( 'NONE',  ( 7.878526806895981061, 20.10277937464278253, -1.676873219709654306 ) ) ;
#8565 = EDGE_CURVE ( 'NONE', #21482, #21386, #2188, .T. ) ;
#8566 = VERTEX_POINT ( 'NONE', #8703 ) ;
#8567 = ORIENTED_EDGE ( 'NONE', *, *, #10696, .T. ) ;
#8568 = DIRECTION ( 'NONE',  ( 0.000000000000000000, 1.000000000000000000, 0.000000000000000000 ) ) ;
#8569 = CARTESIAN_POINT ( 'NONE',  ( 70.64340948846358970, 1.984375000000000000, -10.93409647675949969 ) ) ;
#8570 = AXIS2_PLACEMENT_3D ( 'NONE', #18808, #6881, #11754 ) ;
#8572 = CARTESIAN_POINT ( 'NONE',  ( 12.02474915109715603, -3.968114999999999615, -13.51434638588835391 ) ) ;
#8571 = CARTESIAN_POINT ( 'NONE',  ( 0.8457333743466408649, 11.71888320561318153, 6.611532361588754902 ) ) ;
#8573 = EDGE_LOOP ( 'NONE', ( #8112, #1538, #15065, #18880 ) ) ;
#8574 = CARTESIAN_POINT ( 'NONE',  ( 7.438238543944203585, 17.18978195494404559, 8.325495078195531917 ) ) ;
#8575 = CARTESIAN_POINT ( 'NONE',  ( 1.268730000000000135, 23.41816500000000190, 10.65596716962832069 ) ) ;
#8576 = ORIENTED_EDGE ( 'NONE', *, *, #17803, .T. ) ;
#8577 = ADVANCED_FACE ( 'NONE', ( #12368 ), #20524, .F. ) ;
#8578 = CARTESIAN_POINT ( 'NONE',  ( 0.5166294470163060870, 12.37563144599256226, 3.713427293140974417 ) ) ;
#8579 = AXIS2_PLACEMENT_3D ( 'NONE', #4725, #9463, #17661 ) ;
#8580 = DIRECTION ( 'NONE',  ( 1.000000000000000000, 0.000000000000000000, 0.000000000000000000 ) ) ;
#8581 = EDGE_LOOP ( 'NONE', ( #21875, #9659, #16668, #5526 ) ) ;
#8582 = CARTESIAN_POINT ( 'NONE',  ( 1.992723062505909359, 13.56228047875357845, 1.081925201674736048 ) ) ;
#8583 = CIRCLE ( 'NONE', #11078, 5.357812499999999645 ) ;
#8584 = DIRECTION ( 'NONE',  ( 0.9685006480810793850, 0.000000000000000000, 0.2490110332224846901 ) ) ;
#8585 = DIRECTION ( 'NONE',  ( 0.000000000000000000, 1.000000000000000000, 0.000000000000000000 ) ) ;
#8586 = CARTESIAN_POINT ( 'NONE',  ( 42.35466991749225940, 32.54502000000000095, -17.94967221382040279 ) ) ;
#8587 = CARTESIAN_POINT ( 'NONE',  ( 4.771131690971144756, 20.19041085357579135, 7.102526296929879912 ) ) ;
#8588 = FACE_BOUND ( 'NONE', #14386, .T. ) ;
#8589 = VERTEX_POINT ( 'NONE', #1859 ) ;
#8590 = DIRECTION ( 'NONE',  ( 0.000000000000000000, 1.000000000000000000, 0.000000000000000000 ) ) ;
#8591 = CARTESIAN_POINT ( 'NONE',  ( 55.81697695389291169, 36.51313500000000545, -11.14520323105768362 ) ) ;
#8592 = FILL_AREA_STYLE_COLOUR ( '', #13514 ) ;
#8593 = ADVANCED_FACE ( 'NONE', ( #5608 ), #20303, .T. ) ;
#8595 = CARTESIAN_POINT ( 'NONE',  ( 19.27010264103424930, -5.095940111084548363, -14.21560613677654317 ) ) ;
#8594 = DIRECTION ( 'NONE',  ( -0.9579671649362032637, 0.000000000000000000, 0.2868778675745010664 ) ) ;
#8596 = VECTOR ( 'NONE', #5400, 1000.000000000000000 ) ;
#8597 = EDGE_LOOP ( 'NONE', ( #8374, #2408, #8599, #7350, #12565, #20201, #4958, #891, #21710, #17751, #6230, #18622, #6260, #13138, #11604, #1586, #15759, #10248, #5488, #980, #1991, #9121 ) ) ;
#8598 = EDGE_CURVE ( 'NONE', #4584, #4404, #17016, .T. ) ;
#8599 = ORIENTED_EDGE ( 'NONE', *, *, #5742, .T. ) ;
#8600 = CARTESIAN_POINT ( 'NONE',  ( 6.389564595444752193, 11.61181900198992167, 3.246015655190012339 ) ) ;
#8602 = DIRECTION ( 'NONE',  ( 0.2868778675745011220, 0.000000000000000000, 0.9579671649362034858 ) ) ;
#8601 = CARTESIAN_POINT ( 'NONE',  ( -0.3077843186941259801, 21.11429744052310298, 4.766995793887819133 ) ) ;
#8603 = ORIENTED_EDGE ( 'NONE', *, *, #15751, .F. ) ;
#8604 = ORIENTED_EDGE ( 'NONE', *, *, #11830, .T. ) ;
#8605 = CARTESIAN_POINT ( 'NONE',  ( 1.268730000000000135, 24.21318500000000284, 10.71562499999999929 ) ) ;
#8606 = ORIENTED_EDGE ( 'NONE', *, *, #16985, .T. ) ;
#8607 = CIRCLE ( 'NONE', #18154, 3.175000000000001155 ) ;
#8608 = CARTESIAN_POINT ( 'NONE',  ( 7.449701660363790445, 14.69335886913581213, -1.830007769899437031 ) ) ;
#8609 = DIRECTION ( 'NONE',  ( -0.7334850928793773539, 0.6768732144311022658, 0.06198604769976947398 ) ) ;
#8610 = ORIENTED_EDGE ( 'NONE', *, *, #4694, .T. ) ;
#8611 = CIRCLE ( 'NONE', #17095, 30.16250000000000497 ) ;
#8612 = CARTESIAN_POINT ( 'NONE',  ( 36.54633153140314761, 36.51313500000000545, -9.516661413425623550 ) ) ;
#8613 = DIRECTION ( 'NONE',  ( -0.1831666983862943188, 0.000000000000000000, 0.9830818687180962190 ) ) ;
#8614 = CARTESIAN_POINT ( 'NONE',  ( 0.2150577513804199647, 12.08184417975117242, 2.440174913249124611 ) ) ;
#8615 = CARTESIAN_POINT ( 'NONE',  ( 17.02725982432203367, 128.5105379999999968, -14.27444360421403857 ) ) ;
#8616 = EDGE_LOOP ( 'NONE', ( #11845, #14281, #15393, #3314 ) ) ;
#8617 = CARTESIAN_POINT ( 'NONE',  ( 2.134119274783381925, 14.85629794888722266, 0.06589753127274376732 ) ) ;
#8618 = VECTOR ( 'NONE', #19166, 1000.000000000000227 ) ;
#8619 = CARTESIAN_POINT ( 'NONE',  ( 37.29356535768673098, -6.356984999999999886, -6.700294045292300105 ) ) ;
#8620 = DIRECTION ( 'NONE',  ( 0.5087559856598088404, 0.000000000000000000, 0.8609107660235851833 ) ) ;
#8621 = CARTESIAN_POINT ( 'NONE',  ( 1.173720826352361080, 34.12394749999999988, -20.82884779549221577 ) ) ;
#8622 = CARTESIAN_POINT ( 'NONE',  ( 42.35466991749225940, 32.54502000000000095, -17.94967221382040279 ) ) ;
#8623 = ORIENTED_EDGE ( 'NONE', *, *, #6927, .T. ) ;
#8624 = ADVANCED_FACE ( 'NONE', ( #6843 ), #18879, .F. ) ;
#8625 = CARTESIAN_POINT ( 'NONE',  ( 7.572317812480900301, 20.04452402401122058, -1.518160419548955309 ) ) ;
#8626 = DIRECTION ( 'NONE',  ( 0.000000000000000000, -1.000000000000000000, -0.000000000000000000 ) ) ;
#8627 = CARTESIAN_POINT ( 'NONE',  ( 13.39245492388289982, 15.33820100747184512, 7.095220746324015337 ) ) ;
#8628 = ORIENTED_EDGE ( 'NONE', *, *, #13864, .T. ) ;
#8629 = VECTOR ( 'NONE', #5843, 1000.000000000000000 ) ;
#8630 = ORIENTED_EDGE ( 'NONE', *, *, #4141, .T. ) ;
#8631 = DIRECTION ( 'NONE',  ( 0.000000000000000000, -1.000000000000000000, 0.000000000000000000 ) ) ;
#8632 = CARTESIAN_POINT ( 'NONE',  ( 9.292241171589457949, 17.94623387717348706, 7.752439896407592457 ) ) ;
#8633 = CARTESIAN_POINT ( 'NONE',  ( 0.7904081101278255250, 12.12568132066150106, 4.851017819482066784 ) ) ;
#8634 = DIRECTION ( 'NONE',  ( 0.000000000000000000, 1.000000000000000000, 0.000000000000000000 ) ) ;
#8635 = CARTESIAN_POINT ( 'NONE',  ( 5.651563255009405928, 16.68950339261435545, -1.391004815479667256 ) ) ;
#8636 = LINE ( 'NONE', #16826, #5056 ) ;
#8637 = CARTESIAN_POINT ( 'NONE',  ( 8.359069870979251249, 19.83100852729402064, -1.508148468474054260 ) ) ;
#8638 = CARTESIAN_POINT ( 'NONE',  ( 5.378375181977313346, 15.06312536684776227, 7.861873443265979589 ) ) ;
#8639 = AXIS2_PLACEMENT_3D ( 'NONE', #18664, #3427, #1646 ) ;
#8640 = FACE_OUTER_BOUND ( 'NONE', #206, .T. ) ;
#8641 = CARTESIAN_POINT ( 'NONE',  ( 0.3545653445965538109, 11.62494085263212185, 3.163065520695083066 ) ) ;
#8642 = DIRECTION ( 'NONE',  ( 1.000000000000000000, 0.000000000000000000, 0.000000000000000000 ) ) ;
#8643 = B_SPLINE_CURVE_WITH_KNOTS ( 'NONE', 3,
 ( #5686, #3928, #12447, #2701, #9000, #2260 ),
 .UNSPECIFIED., .F., .F.,
 ( 4, 1, 1, 4 ),
 ( 0.4992858149431267933, 0.5000000202745523703, 0.7500007535597175146, 1.000000000000000000 ),
 .UNSPECIFIED. ) ;
#8644 = CARTESIAN_POINT ( 'NONE',  ( 19.67909734877197891, 0.1298811790940870847, -14.89708569419555317 ) ) ;
#8645 = CARTESIAN_POINT ( 'NONE',  ( 6.452480818898766124, 10.92909956722771092, 2.773400309299709043 ) ) ;
#8646 = CARTESIAN_POINT ( 'NONE',  ( 39.07078961959606289, 0.000000000000000000, -27.14892015257980162 ) ) ;
#8647 = CARTESIAN_POINT ( 'NONE',  ( 17.89770978039528515, -8.066346848044377182, -15.66321486863013490 ) ) ;
#8648 = DIRECTION ( 'NONE',  ( -0.9790635044817341814, 0.000000000000000000, 0.2035550397114869736 ) ) ;
#8649 = EDGE_CURVE ( 'NONE', #4259, #6430, #8929, .T. ) ;
#8650 = CARTESIAN_POINT ( 'NONE',  ( 9.458380351582428958, 21.87037480992658089, 2.696715734057056668 ) ) ;
#8651 = VERTEX_POINT ( 'NONE', #20637 ) ;
#8652 = CARTESIAN_POINT ( 'NONE',  ( 11.15553486249665482, 14.64160775519011182, -3.299033682045386495 ) ) ;
#8653 = CARTESIAN_POINT ( 'NONE',  ( 19.12821060939544182, -0.2463727629768049099, -14.53839379697989465 ) ) ;
#8655 = CARTESIAN_POINT ( 'NONE',  ( 49.81956284419040060, 30.56064500000000095, 11.98436472153758103 ) ) ;
#8654 = CARTESIAN_POINT ( 'NONE',  ( 1.003497587984025108, 20.41800832758468331, 3.587532134645925908 ) ) ;
#8656 = ORIENTED_EDGE ( 'NONE', *, *, #9518, .F. ) ;
#8657 = APPLICATION_PROTOCOL_DEFINITION ( 'draft international standard', 'automotive_design', 1998, #983 ) ;
#8658 = VECTOR ( 'NONE', #3622, 1000.000000000000000 ) ;
#8659 = DIRECTION ( 'NONE',  ( 0.000000000000000000, 1.000000000000000000, 0.000000000000000000 ) ) ;
#8660 = LINE ( 'NONE', #11988, #16411 ) ;
#8661 = CARTESIAN_POINT ( 'NONE',  ( 21.26384696840964494, -2.656554757447519677, -14.29854077623973296 ) ) ;
#8662 = ORIENTED_EDGE ( 'NONE', *, *, #68, .F. ) ;
#8663 = CARTESIAN_POINT ( 'NONE',  ( 10.28589934229847280, 11.26381867368412060, 2.184127149925467748 ) ) ;
#8664 = EDGE_CURVE ( 'NONE', #1990, #13930, #424, .T. ) ;
#8665 = CARTESIAN_POINT ( 'NONE',  ( 6.854702814278667233, 12.02528521847468213, 4.767674869364597612 ) ) ;
#8666 = CARTESIAN_POINT ( 'NONE',  ( 0.5698505877279143039, 20.87305502788824185, 6.283888600290745252 ) ) ;
#8667 = CARTESIAN_POINT ( 'NONE',  ( 12.12410201198690629, 21.60500416633145804, -1.540977856777658639 ) ) ;
#8668 = DIRECTION ( 'NONE',  ( 0.2490110332224846623, 0.000000000000000000, -0.9685006480810793850 ) ) ;
#8669 = CARTESIAN_POINT ( 'NONE',  ( 15.51594691092190281, 1.079619396839424539, -15.60350270339164602 ) ) ;
#8670 = CARTESIAN_POINT ( 'NONE',  ( 10.72409186464205355, -4.809670885807086016, -15.96177715662992824 ) ) ;
#8671 = EDGE_CURVE ( 'NONE', #9683, #9903, #5172, .T. ) ;
#8672 = ORIENTED_EDGE ( 'NONE', *, *, #872, .F. ) ;
#8673 = EDGE_CURVE ( 'NONE', #21216, #4173, #10709, .T. ) ;
#8674 = CARTESIAN_POINT ( 'NONE',  ( 7.740651597158667130, 11.34324505471928113, -0.1322639018746852579 ) ) ;
#8675 = ORIENTED_EDGE ( 'NONE', *, *, #21417, .F. ) ;
#8676 = CARTESIAN_POINT ( 'NONE',  ( 30.02465935949302533, 2.019535839764540430, -2.324128137548288731 ) ) ;
#8677 = DIRECTION ( 'NONE',  ( -0.2868778675745011220, 0.000000000000000000, -0.9579671649362034858 ) ) ;
#8679 = DIRECTION ( 'NONE',  ( -0.2490110332224889089, -7.284927983104707832E-16, 0.9685006480810781637 ) ) ;
#8678 = CARTESIAN_POINT ( 'NONE',  ( 0.5238767203945161599, 20.13149037663900387, 7.903974376171220229 ) ) ;
#8680 = ORIENTED_EDGE ( 'NONE', *, *, #3564, .F. ) ;
#8681 = CARTESIAN_POINT ( 'NONE',  ( 7.064467163856848586, 11.61461761587226249, 5.722166049371485208 ) ) ;
#8682 = PLANE ( 'NONE',  #18991 ) ;
#8683 = ORIENTED_EDGE ( 'NONE', *, *, #10600, .F. ) ;
#8684 = DIRECTION ( 'NONE',  ( 0.000000000000000000, 0.000000000000000000, -1.000000000000000000 ) ) ;
#8685 = ORIENTED_EDGE ( 'NONE', *, *, #20965, .F. ) ;
#8686 = EDGE_CURVE ( 'NONE', #13702, #6259, #201, .T. ) ;
#8687 = DIRECTION ( 'NONE',  ( 0.000000000000000000, -1.000000000000000000, 0.000000000000000000 ) ) ;
#8688 = CARTESIAN_POINT ( 'NONE',  ( 32.04318496342826705, -6.356984999999999886, -2.596378499983996946 ) ) ;
#8689 = CARTESIAN_POINT ( 'NONE',  ( 44.28293121686854761, 36.51313500000000545, -31.08068102505560759 ) ) ;
#8690 = CARTESIAN_POINT ( 'NONE',  ( 4.731467607026393907, 20.28102513395944229, 7.000553450486113327 ) ) ;
#8691 = DIRECTION ( 'NONE',  ( 0.000000000000000000, -1.000000000000000000, 0.000000000000000000 ) ) ;
#8692 = ORIENTED_EDGE ( 'NONE', *, *, #14371, .F. ) ;
#8693 = ADVANCED_FACE ( 'NONE', ( #308 ), #15585, .F. ) ;
#8694 = DIRECTION ( 'NONE',  ( 0.000000000000000000, 1.000000000000000000, 0.000000000000000000 ) ) ;
#8695 = FACE_OUTER_BOUND ( 'NONE', #11568, .T. ) ;
#8696 = FACE_OUTER_BOUND ( 'NONE', #14178, .T. ) ;
#8698 = CARTESIAN_POINT ( 'NONE',  ( 15.00318546702699152, -7.179718225927687492, -15.07128219575455219 ) ) ;
#8697 = CARTESIAN_POINT ( 'NONE',  ( 52.44708915697334106, 32.54502000000000095, 4.020247972991190188 ) ) ;
#8699 = ORIENTED_EDGE ( 'NONE', *, *, #3894, .F. ) ;
#8700 = VERTEX_POINT ( 'NONE', #10378 ) ;
#8701 = CARTESIAN_POINT ( 'NONE',  ( 8.492895593974109758, 11.54146397052094208, 3.562534344333246228 ) ) ;
#8703 = CARTESIAN_POINT ( 'NONE',  ( 12.79472653632228507, 34.52875999999999834, -13.31637763425449883 ) ) ;
#8702 = CARTESIAN_POINT ( 'NONE',  ( 1.814661426025774071, 13.02131026627836086, 0.3805811478219760513 ) ) ;
#8704 = ORIENTED_EDGE ( 'NONE', *, *, #12768, .T. ) ;
#8705 = CARTESIAN_POINT ( 'NONE',  ( 4.607010772665877774, 11.08493650962506116, 3.903497619132711094 ) ) ;
#8706 = ADVANCED_FACE ( 'NONE', ( #12259 ), #5273, .F. ) ;
#8707 = ORIENTED_EDGE ( 'NONE', *, *, #18123, .F. ) ;
#8708 = CARTESIAN_POINT ( 'NONE',  ( -3.042350287543033716, 26.98019749999999917, -26.17378113315171007 ) ) ;
#8709 = AXIS2_PLACEMENT_3D ( 'NONE', #19336, #17914, #2760 ) ;
#8710 = ORIENTED_EDGE ( 'NONE', *, *, #13409, .T. ) ;
#8711 = CARTESIAN_POINT ( 'NONE',  ( 7.633935190542764815, 17.76945892008578198, -1.936471469497620390 ) ) ;
#8712 = ORIENTED_EDGE ( 'NONE', *, *, #3615, .T. ) ;
#8713 = CARTESIAN_POINT ( 'NONE',  ( 3.412213502827448064, 15.93234797188829432, 8.430948932171904886 ) ) ;
#8714 = ADVANCED_FACE ( 'NONE', ( #8808 ), #18982, .T. ) ;
#8715 = EDGE_CURVE ( 'NONE', #19210, #15662, #14044, .T. ) ;
#8716 = EDGE_CURVE ( 'NONE', #18111, #13681, #12410, .T. ) ;
#8717 = CARTESIAN_POINT ( 'NONE',  ( 30.86636926788154156, 3.565842500000000914, -42.59335521360503662 ) ) ;
#8718 = CARTESIAN_POINT ( 'NONE',  ( 47.80475250345343596, 37.69740999999999786, -11.91473563638196786 ) ) ;
#8719 = CARTESIAN_POINT ( 'NONE',  ( 3.289252607606479195, 18.65028268025089275, 8.659271349972804899 ) ) ;
#8720 = DIRECTION ( 'NONE',  ( 0.2868778675745011220, 0.000000000000000000, 0.9579671649362034858 ) ) ;
#8721 = AXIS2_PLACEMENT_3D ( 'NONE', #13247, #6587, #8243 ) ;
#8722 = ORIENTED_EDGE ( 'NONE', *, *, #10148, .F. ) ;
#8723 = CARTESIAN_POINT ( 'NONE',  ( 0.2840622119934582135, 15.69350566183319273, 0.5951328775468103238 ) ) ;
#8724 = CARTESIAN_POINT ( 'NONE',  ( 39.27728671717661513, 34.52875999999999834, -23.95520057284206672 ) ) ;
#8725 = DIRECTION ( 'NONE',  ( 0.000000000000000000, 1.000000000000000000, 0.000000000000000000 ) ) ;
#8726 = CARTESIAN_POINT ( 'NONE',  ( 23.00195419928544638, 3.565842500000000914, -15.19829965147284945 ) ) ;
#8727 = VERTEX_POINT ( 'NONE', #20859 ) ;
#8728 = CARTESIAN_POINT ( 'NONE',  ( 8.475013748165151739, 20.13899192311416186, 6.625161462038594351 ) ) ;
#8729 = LINE ( 'NONE', #17032, #19815 ) ;
#8730 = CARTESIAN_POINT ( 'NONE',  ( 12.87833794687879774, 19.58183286683828683, 6.222496348469165994 ) ) ;
#8731 = ORIENTED_EDGE ( 'NONE', *, *, #6622, .F. ) ;
#8732 = ORIENTED_EDGE ( 'NONE', *, *, #7459, .F. ) ;
#8733 = CARTESIAN_POINT ( 'NONE',  ( 12.88040283537677588, 13.08893749999999834, -0.09070320285213756550 ) ) ;
#8734 = CARTESIAN_POINT ( 'NONE',  ( 8.646429374176550553, 10.88129523880938088, 3.767012232034312458 ) ) ;
#8735 = CARTESIAN_POINT ( 'NONE',  ( 0.03748398651459098480, 15.70515029433102860, 0.7586468221082122154 ) ) ;
#8736 = DIRECTION ( 'NONE',  ( 0.000000000000000000, 0.000000000000000000, -1.000000000000000000 ) ) ;
#8737 = CARTESIAN_POINT ( 'NONE',  ( 6.194255370365423730, 19.41116075945178920, -0.3004728795146091036 ) ) ;
#8738 = CARTESIAN_POINT ( 'NONE',  ( -19.26432987443570966, -5.953760000000000829, -73.22178168742661342 ) ) ;
#8739 = EDGE_CURVE ( 'NONE', #1050, #19416, #745, .T. ) ;
#8740 = CARTESIAN_POINT ( 'NONE',  ( 2.370064745689808294, 19.81445010932126038, 0.4253065698170983011 ) ) ;
#8741 = DIRECTION ( 'NONE',  ( 0.6702301885068632226, 0.000000000000000000, 0.7421532822901576454 ) ) ;
#8742 = CARTESIAN_POINT ( 'NONE',  ( 19.96125241592742938, -0.3821940830726566762, -14.83098244249484310 ) ) ;
#8743 = CARTESIAN_POINT ( 'NONE',  ( 3.427273626668901230, 14.96908372069038684, 8.327090403724351830 ) ) ;
#8744 = DIRECTION ( 'NONE',  ( 0.000000000000000000, 0.000000000000000000, -1.000000000000000000 ) ) ;
#8745 = DIRECTION ( 'NONE',  ( 0.000000000000000000, 1.000000000000000000, 0.000000000000000000 ) ) ;
#8746 = CARTESIAN_POINT ( 'NONE',  ( 17.39231329963745409, -8.234078972146175346, -15.77331051030036235 ) ) ;
#8747 = CARTESIAN_POINT ( 'NONE',  ( 26.59062499999999929, 26.59189500000000095, 10.71562499999999929 ) ) ;
#8748 = DIRECTION ( 'NONE',  ( 0.6702301885068630005, 0.000000000000000000, 0.7421532822901579785 ) ) ;
#8749 = CARTESIAN_POINT ( 'NONE',  ( 11.43397512567650942, 15.80362715008215524, 7.556022402886738654 ) ) ;
#8750 = CYLINDRICAL_SURFACE ( 'NONE', #20506, 0.5079999999999995630 ) ;
#8752 = CARTESIAN_POINT ( 'NONE',  ( 11.54900921193965857, 11.99113680707610996, -1.243656623600980504 ) ) ;
#8751 = B_SPLINE_CURVE_WITH_KNOTS ( 'NONE', 3,
 ( #9553, #13010, #12568, #2384, #14444, #14675, #4153, #9111, #7580, #938, #21057, #16108, #21161, #19291, #15894, #17864, #1159, #7898, #7468, #21382, #21275, #6131, #5908, #835, #20956, #14239, #12900, #5812, #19614, #6237, #9336, #2710, #10891, #2492, #6016, #17758, #19392, #17640, #9224, #16006, #4262, #2606, #12788, #19511, #4481, #4377, #14556, #11113, #9444, #16216, #1043, #7788, #11217, #17968, #2818, #17349, #18989, #14270, #643, #19424, #20645, #14053, #869, #5616, #5737, #5839, #19102, #2304, #2417, #14161, #15816, #19215, #752, #4183, #17676, #9257, #14922, #3076, #4737, #6169, #13263, #4413, #12934, #16137, #18113, #6052, #14478, #21193, #16353, #7936, #12823, #19642, #1192, #9697, #21522, #8037, #6380, #15241, #8578, #18860, #6922, #15132, #6818, #13363, #10356, #15031, #5152, #20070, #12012, #17100, #15459, #5051, #13578, #9907, #16673, #12133, #11687, #10028, #6708, #17545, #19191, #7478, #12576, #17438, #10571, #12346, #4057, #19299, #10901, #2394, #13919, #19072, #5916, #9123, #3727, #2044, #402, #5478, #12237, #17316, #1167, #1374, #9454, #1053, #8115, #16442, #21615, #9346, #6142, #6474, #4275, #16115, #12912, #14454, #2828, #7907, #21391, #18088, #8015, #2946, #13125, #14785, #10182, #18911, #571, #11958, #16926, #235, #17157, #13743, #3671, #10516, #3556, #15632, #19947, #7215, #17385, #5310, #20674, #124, #12292, #1775, #10296, #15845, #9177, #11069, #16066, #7535, #19347, #995, #12734, #16169, #20901, #10954, #5865, #19457, #2668, #19139, #9401, #6083, #2771, #12855, #9507, #11171, #11721, #8065, #12962, #14732, #11279, #15059, #8178, #21771, #13289, #13388, #6293, #21553, #14953, #18455, #10057, #4540, #16381, #19890, #18141, #13071, #19776, #15274, #3865, #8713, #433, #7185, #1643, #20648, #12163, #3424, #13497, #1974, #13718, #5507, #8821, #17134, #100, #13610, #320, #3757, #17235, #15596, #17679, #2420, #19217, #9041, #543, #20866, #7717, #10720, #11040, #9372, #14373, #10821, #12702, #12379, #16038, #21088, #5937, #12826, #17569, #9147, #7505, #14273, #16248, #19972, #11366, #14599, #19866, #3079, #21749, #8039, #19645, #19748, #7938, #21415, #4621, #6270, #18116, #1403, #2972, #8146, #21642, #11583, #1518, #17205, #7029, #15135, #10239, #6821, #8582, #12015, #4939, #21854, #6712, #11804, #7158, #3401, #1841, #181, #20390, #17103, #1943, #15463, #7594, #3838, #20969, #17321, #17656, #2505, #2619, #9350, #16120, #5482, #20735, #5590, #12351, #19076, #2283, #9021, #12471, #4061, #17549, #7697, #1276, #11558, #9881, #4492, #14458, #19726, #4599, #2724, #2832, #14789, #9458, #1056, #14577, #1173, #7914, #13130, #4717, #9779, #14900, #6478, #6795, #1493, #15332, #7006, #13553, #16962, #6684, #1919, #156, #20365, #6900, #10332, #20048, #13664, #18511, #11992, #10110, #18720, #1700, #8441, #20813, #3922, #2256, #3809, #7128, #9207, #15544, #376, #8882, #20707, #598, #7566, #13896, #12218, #5562, #19170, #14328, #15875, #5893, #16416, #4684, #2698, #11202, #19698, #6443, #21365, #9648, #21145, #19809, #7884, #9323, #18058, #9751, #16096, #2918, #7669, #19495, #16201, #6116, #14762, #21468, #21697, #3452, #4995, #8638, #18690, #11752, #241, #18369, #127, #13747, #10084, #4793, #13639, #9975, #16733, #15085, #6651, #20339, #16829, #18806, #7095, #20444, #10418, #13862, #7220, #5427, #12191, #8853, #12526, #576, #2338, #15848, #15636, #20678, #3896, #14081, #10636, #676, #20906, #4110, #18223, #2975, #9803, #14930, #19749, #14601, #6505, #4941, #11692, #12936, #10035, #13368, #17998, #16466, #8040, #16356, #2855, #4623, #6386, #19867, #11585, #3179, #10360, #2048, #13583, #18749, #15357, #10241, #8468, #11807, #15245, #21855, #13690, #1945, #20184, #18538, #15465, #7030, #3731, #6348, #1693, #8231, #16439, #18503, #10105, #21609, #19944, #8431, #3050, #1269, #8012, #11657, #3266, #4710, #18289, #16538, #13235, #4818, #15005, #21822, #16952, #14000, #20256, #2017, #151, #10540, #3805, #5557, #15433, #6999, #18607, #13657, #5337, #370, #13890, #20359, #3582, #10659, #2132, #8989, #20587, #20934, #5792, #17736, #9425, #12766, #19375, #19164, #4130, #4356, #9317, #10871, #17620, #1023, #2798, #921, #11197, #14426, #2362, #9201, #6109, #11519, #11748, #9969, #2913, #11630, #12986, #9643, #4990, #6439, #21360, #18478, #3022, #18261, #4565, #19805, #14758, #16509, #1568, #9846, #1457, #8310, #1996, #3349, #12073, #13976, #15629, #15300, #10080, #234, #20439, #15181, #12187, #17262, #2106, #20333, #10294, #6759, #11854, #18583, #6875, #5308, #2448, #4214, #9175, #15742, #10952, #7314, #15956, #12624, #20786, #11068, #12732, #787, #5649, #9290, #17825, #17491, #2334, #9068, #6529, #21550, #11606, #14627, #1321, #7963, #4650, #19669, #1219, #16592, #21770, #15058, #11394, #19575, #4441, #16702, #14835, #13181, #4763, #18342, #17923, #17012 ),
 .UNSPECIFIED., .F., .F.,
 ( 4, 3, 3, 3, 3, 3, 3, 3, 3, 3, 3, 3, 3, 3, 3, 3, 3, 3, 3, 3, 3, 3, 3, 3, 3, 3, 3, 3, 3, 3, 3, 3, 3, 3, 3, 3, 3, 3, 3, 3, 3, 3, 3, 3, 3, 3, 3, 3, 3, 3, 3, 3, 3, 3, 3, 3, 3, 3, 3, 3, 3, 3, 3, 3, 3, 3, 3, 3, 3, 3, 3, 3, 3, 3, 3, 3, 3, 3, 3, 3, 3, 3, 3, 3, 3, 3, 3, 3, 3, 3, 3, 3, 3, 3, 3, 3, 3, 3, 3, 3, 3, 3, 3, 3, 3, 3, 3, 3, 3, 3, 3, 3, 3, 3, 3, 3, 3, 3, 3, 3, 3, 3, 3, 3, 3, 3, 3, 3, 3, 3, 3, 3, 3, 3, 3, 3, 3, 3, 3, 3, 3, 3, 3, 3, 3, 3, 3, 3, 3, 3, 3, 3, 3, 3, 3, 3, 3, 3, 3, 3, 3, 3, 3, 3, 3, 3, 3, 3, 3, 3, 3, 3, 3, 3, 3, 3, 3, 3, 3, 3, 3, 3, 3, 3, 3, 3, 3, 3, 3, 3, 3, 3, 3, 3, 3, 3, 3, 3, 3, 3, 3, 3, 3, 3, 3, 3, 3, 3, 3, 3, 4 ),
 ( 0.000000000000000000, 0.006578947365780970537, 0.01249999562829610077, 0.01315789473155989930, 0.01973684209733990100, 0.02631578946311990269, 0.02875001438670990103, 0.03289473682890979578, 0.03947368419468980094, 0.04499999191018719952, 0.04605263156046980610, 0.05263157892624970025, 0.05921052629202970541, 0.06125001564970669610, 0.06578947365780969669, 0.07236842102358960471, 0.07749998933833390780, 0.07894736838936959600, 0.08552631575514958728, 0.09210526312092949530, 0.09375001447617459238, 0.09868421048671950635, 0.1052631578524590023, 0.1099999887899340001, 0.1118421052183189990, 0.1184210525840789924, 0.1249999999498389996, 0.1262500112023720034, 0.1315789473155989930, 0.1381578946813590003, 0.1424999906499269942, 0.1447368420472190109, 0.1513157894129790182, 0.1578947367787389977, 0.1587500068096430184, 0.1644736841444989772, 0.1710526315102589845, 0.1749999946880989865, 0.1776315788761189951, 0.1842105262418790024, 0.1907894736076390096, 0.1912500026574869838, 0.1973684209733990169, 0.2039473683392589998, 0.2075000001683630080, 0.2105263157050190070, 0.2171052630707789866, 0.2236842104365389938, 0.2302631578022990011, 0.2368421051681589840, 0.2400000060332939944, 0.2434210525339189912, 0.2499999998996789985, 0.2562499982428639855, 0.2565789472654390058, 0.2631578946311989853, 0.2697368419970589959, 0.2725000111344089704, 0.2763157893628189754, 0.2828947367285789549, 0.2887499948061880151, 0.2894736840943389899, 0.2960526314600980258, 0.3026315788259580364, 0.3050000144739509755, 0.3092105261917179604, 0.3157894735574779954, 0.3212499912461020402, 0.3223684209232379749, 0.3289473682890980410, 0.3355263156548580206, 0.3375000154242109862, 0.3421052630206180001, 0.3486842103863779796, 0.3537499889259840269, 0.3552631577521380146, 0.3618421051179980252, 0.3684210524837580047, 0.3700000138896000212, 0.3749999998495179843, 0.3815789472152780193, 0.3862499887360519857, 0.3881578945810379988, 0.3947368419468980094, 0.4013157893126579889, 0.4025000103777250371, 0.4078947366784179684, 0.4144736840441780035, 0.4187499909580220114, 0.4210526314099379830, 0.4276315787757979936, 0.4342105261415579731, 0.4350000059446500478, 0.4407894735073180081, 0.4473684208730779877, 0.4512499952738350251, 0.4539473682389379983, 0.4605263156046980333, 0.4671052629704580128, 0.4675000019802649787, 0.4736842103362179923, 0.4802631577019779718, 0.4837500008840890375, 0.4868421050678370388, 0.4934210524335980175, 0.4999999997993569978, 0.5065789471651169773, 0.5131578945308770123, 0.5162500067017939953, 0.5197368418967369674, 0.5263157892624970025, 0.5324999976354098941, 0.5328947366282570375, 0.5394736839940169615, 0.5460526313597769965, 0.5487500115865550088, 0.5526315787256369516, 0.5592105260913969866, 0.5649999940639039986, 0.5657894734571570217, 0.5723684208229169457, 0.5789473681887770118, 0.5812500145853020106, 0.5855263155545369358, 0.5921052629202969708, 0.5974999906071669642, 0.5986842102860570058, 0.6052631576518170409, 0.6118421050176769960, 0.6137500151446890762, 0.6184210523834369200, 0.6249999997491970660, 0.6299999885682440182, 0.6315789471149569900, 0.6381578944807170251, 0.6447368418465769802, 0.6462500132616529891, 0.6513157892123370152, 0.6578947365780970502, 0.6624999887461079373, 0.6644736839438569742, 0.6710526313096170092, 0.6776315786754769643, 0.6787500095369500830, 0.6842105260412369994, 0.6907894734069960352, 0.6949999913246359684, 0.6973684207727559592, 0.7039473681386160253, 0.7105263155043759493, 0.7112500050977950128, 0.7171052628701359843, 0.7236842102358960194, 0.7274999959004379013, 0.7302631576016559434, 0.7368421049675160095, 0.7434210523332759335, 0.7437500013550489841, 0.7499999996990360795, 0.7565789470647958925, 0.7600000016152699267, 0.7631578944305560386, 0.7697368417964159937, 0.7763157891621760287, 0.7828947365279360637, 0.7894736838936959877, 0.7925000073580670268, 0.7960526312594560228, 0.8026315786253159779, 0.8087499969874719641, 0.8092105259910760129, 0.8157894733568360479, 0.8223684207225959719, 0.8250000120025489103, 0.8289473680884560380, 0.8355263154542159620, 0.8412499933217569836, 0.8421052628199759971, 0.8486842101857360321, 0.8552631575514959561, 0.8575000146455890038, 0.8618421049173560222, 0.8684210522831159462, 0.8737499900031009403, 0.8749999996488759813, 0.8815789470146359053, 0.8881578943803950521, 0.8900000148124059818, 0.8947368417462548962, 0.9013157891120149312, 0.9062499882679529994, 0.9078947364777750773, 0.9144736838435350013, 0.9210526312092950363, 0.9225000125942429685, 0.9276315785751549914, 0.9342105259409150264, 0.9387499888219880129, 0.9407894733066750614, 0.9473684206724349854, 0.9539473680382950516, 0.9550000086894259166, 0.9605263154040549756, 0.9671052627698150106, 0.9712499916671659683, 0.9736842101355750456, 0.9802631575013349696, 0.9868421048671950357, 0.9875000041866580647, 0.9934210522329549597, 0.9999999995987149948 ),
 .UNSPECIFIED. ) ;
#8753 = DIRECTION ( 'NONE',  ( -0.9685006480810794960, 0.000000000000000000, -0.2490110332224836354 ) ) ;
#8755 = DIRECTION ( 'NONE',  ( 0.000000000000000000, 1.000000000000000000, 0.000000000000000000 ) ) ;
#8754 = CARTESIAN_POINT ( 'NONE',  ( 4.216071159329941587, 19.96663567226219982, 0.9010242342158106821 ) ) ;
#8756 = ORIENTED_EDGE ( 'NONE', *, *, #6925, .F. ) ;
#8757 = APPLICATION_PROTOCOL_DEFINITION ( 'draft international standard', 'automotive_design', 1998, #11877 ) ;
#8758 = DIRECTION ( 'NONE',  ( -0.000000000000000000, -1.000000000000000000, 0.000000000000000000 ) ) ;
#8759 = FACE_OUTER_BOUND ( 'NONE', #13153, .T. ) ;
#8760 = CARTESIAN_POINT ( 'NONE',  ( 53.14266576735293768, -5.167590446840315543, -16.66242751532468702 ) ) ;
#8761 = EDGE_CURVE ( 'NONE', #17518, #5857, #21556, .T. ) ;
#8762 = AXIS2_PLACEMENT_3D ( 'NONE', #1655, #21785, #13397 ) ;
#8763 = EDGE_LOOP ( 'NONE', ( #2572, #21674, #11778, #19942, #12920 ) ) ;
#8764 = CARTESIAN_POINT ( 'NONE',  ( 5.703757595802129821, 13.98659666219624675, -0.8855850056449419139 ) ) ;
#8765 = CARTESIAN_POINT ( 'NONE',  ( 9.580014628452152792, 12.37431098505726013, -1.091745231617962997 ) ) ;
#8766 = CARTESIAN_POINT ( 'NONE',  ( 7.883452240851667625, 14.83344068326428022, 7.768530631985846924 ) ) ;
#8767 = CARTESIAN_POINT ( 'NONE',  ( 10.28446018311015742, 10.45470314796870248, 2.211657637955910083 ) ) ;
#8768 = CARTESIAN_POINT ( 'NONE',  ( 46.07940063401251507, 32.54502000000000095, -26.08707253294707229 ) ) ;
#8769 = VECTOR ( 'NONE', #5788, 1000.000000000000114 ) ;
#8770 = CARTESIAN_POINT ( 'NONE',  ( 12.55470403860302753, -0.7187473132079236215, -16.53897826650729286 ) ) ;
#8771 = UNCERTAINTY_MEASURE_WITH_UNIT (LENGTH_MEASURE( 1.000000000000000082E-05 ), #19730, 'distance_accuracy_value', 'NONE');
#8772 = FACE_OUTER_BOUND ( 'NONE', #12318, .T. ) ;
#8773 = VERTEX_POINT ( 'NONE', #9138 ) ;
#8774 = CARTESIAN_POINT ( 'NONE',  ( 11.09769854542326861, 17.23211763628403403, 6.743335639867776621 ) ) ;
#8775 = CARTESIAN_POINT ( 'NONE',  ( 11.14235852144809868, 12.31819272753022254, -2.976272612453031652 ) ) ;
#8776 = ORIENTED_EDGE ( 'NONE', *, *, #362, .F. ) ;
#8777 = CARTESIAN_POINT ( 'NONE',  ( 10.69018650721368502, 11.75921469276450182, 3.871793181027931574 ) ) ;
#8778 = CIRCLE ( 'NONE', #1728, 25.00312500000000426 ) ;
#8779 = LINE ( 'NONE', #18848, #3868 ) ;
#8780 = CARTESIAN_POINT ( 'NONE',  ( 12.94499384098450001, 22.19916506436698000, 0.6856174611774060734 ) ) ;
#8782 = CARTESIAN_POINT ( 'NONE',  ( -17.46249999999999858, 33.73373999999999739, 0.000000000000000000 ) ) ;
#8781 = CARTESIAN_POINT ( 'NONE',  ( 1.162433488273821647, 12.61021756743670252, 8.063620084594539605 ) ) ;
#8783 = ORIENTED_EDGE ( 'NONE', *, *, #8150, .T. ) ;
#8784 = CARTESIAN_POINT ( 'NONE',  ( 6.437478173552243277, 10.90738268085100060, 3.037243646032500521 ) ) ;
#8785 = CARTESIAN_POINT ( 'NONE',  ( 24.60624999999999929, 16.27314499999999953, 10.71562499999999929 ) ) ;
#8786 = ORIENTED_EDGE ( 'NONE', *, *, #9786, .T. ) ;
#8787 = AXIS2_PLACEMENT_3D ( 'NONE', #16613, #11515, #21461 ) ;
#8788 = EDGE_CURVE ( 'NONE', #9986, #14245, #17562, .T. ) ;
#8789 = DIRECTION ( 'NONE',  ( -0.8667647648559581031, 0.000000000000000000, -0.4987171968201974948 ) ) ;
#8790 = EDGE_LOOP ( 'NONE', ( #16139, #9695, #4343, #17303, #10726, #8197, #417, #154, #21571, #9958, #1076, #1931 ) ) ;
#8791 = ADVANCED_FACE ( 'NONE', ( #5730 ), #11242, .F. ) ;
#8792 = CARTESIAN_POINT ( 'NONE',  ( 34.38097451710952868, 34.52875999999999834, 0.2081255904771098786 ) ) ;
#8793 = FACE_OUTER_BOUND ( 'NONE', #14907, .T. ) ;
#8794 = LINE ( 'NONE', #12354, #15766 ) ;
#8795 = CARTESIAN_POINT ( 'NONE',  ( 5.416218533946238090, 17.73239028602085199, 8.614334791690790638 ) ) ;
#8796 = LINE ( 'NONE', #12142, #8360 ) ;
#8797 = VERTEX_POINT ( 'NONE', #635 ) ;
#8798 = CIRCLE ( 'NONE', #16249, 0.7950200000000000600 ) ;
#8799 = CARTESIAN_POINT ( 'NONE',  ( 17.30373842852263877, 34.52875999999999834, -12.15706637069277107 ) ) ;
#8800 = DIRECTION ( 'NONE',  ( 0.9685006480810791629, 0.000000000000000000, 0.2490110332224850231 ) ) ;
#8801 = DIRECTION ( 'NONE',  ( 0.000000000000000000, 0.000000000000000000, 1.000000000000000000 ) ) ;
#8803 = CARTESIAN_POINT ( 'NONE',  ( 11.81489480681374715, -4.423560566030090513, -15.68132100509055782 ) ) ;
#8802 = LINE ( 'NONE', #2180, #14462 ) ;
#8804 = ORIENTED_EDGE ( 'NONE', *, *, #12135, .T. ) ;
#8805 = VERTEX_POINT ( 'NONE', #2412 ) ;
#8806 = CARTESIAN_POINT ( 'NONE',  ( 13.42753679035789105, 21.40794255445344163, 2.286611137732273757 ) ) ;
#8808 = FACE_OUTER_BOUND ( 'NONE', #12667, .T. ) ;
#8807 = CARTESIAN_POINT ( 'NONE',  ( 1.708238430344685144, 13.92071940861192658, 9.099522166506517351 ) ) ;
#8809 = ORIENTED_EDGE ( 'NONE', *, *, #8149, .T. ) ;
#8811 = CARTESIAN_POINT ( 'NONE',  ( 11.44793084563043095, -6.323609490084446172, -16.58140058502533520 ) ) ;
#8810 = CARTESIAN_POINT ( 'NONE',  ( 4.373404510246160726, 11.14075155979819165, 2.905983407409085117 ) ) ;
#8812 = EDGE_CURVE ( 'NONE', #12648, #7062, #13467, .T. ) ;
#8813 = EDGE_LOOP ( 'NONE', ( #16256, #9089, #8036, #10255 ) ) ;
#8814 = AXIS2_PLACEMENT_3D ( 'NONE', #13231, #19941, #4814 ) ;
#8815 = VERTEX_POINT ( 'NONE', #19207 ) ;
#8816 = CARTESIAN_POINT ( 'NONE',  ( 7.721685948793786558, 12.55088109015116693, -0.3031984390922063399 ) ) ;
#8817 = EDGE_CURVE ( 'NONE', #3064, #1375, #12762, .T. ) ;
#8818 = ORIENTED_EDGE ( 'NONE', *, *, #6643, .T. ) ;
#8819 = EDGE_CURVE ( 'NONE', #18667, #11600, #19095, .T. ) ;
#8820 = AXIS2_PLACEMENT_3D ( 'NONE', #17935, #9515, #16285 ) ;
#8821 = CARTESIAN_POINT ( 'NONE',  ( 3.407061386797684666, 14.37727598515552607, 7.987795225252861897 ) ) ;
#8822 = CIRCLE ( 'NONE', #3500, 0.7950200000000000600 ) ;
#8823 = LINE ( 'NONE', #438, #15969 ) ;
#8824 = CARTESIAN_POINT ( 'NONE',  ( 38.84151346225866774, -7.551139666418512419, -4.076215976391670992 ) ) ;
#8825 = DIRECTION ( 'NONE',  ( 0.9876802608827758290, 0.000000000000000000, -0.1564854698127972066 ) ) ;
#8826 = DIRECTION ( 'NONE',  ( -0.8609107660235848503, 0.000000000000000000, 0.5087559856598096175 ) ) ;
#8827 = CARTESIAN_POINT ( 'NONE',  ( 3.515735123799623274, 17.35852335215787789, 9.108230659777527549 ) ) ;
#8828 = FACE_BOUND ( 'NONE', #4018, .T. ) ;
#8829 = CIRCLE ( 'NONE', #3197, 30.16249999999998721 ) ;
#8830 = VERTEX_POINT ( 'NONE', #2735 ) ;
#8831 = CARTESIAN_POINT ( 'NONE',  ( 5.343034057657806812, 20.72645064840772022, 2.101598573111083113 ) ) ;
#8832 = DIRECTION ( 'NONE',  ( -0.6702301885068628895, 0.000000000000000000, -0.7421532822901579785 ) ) ;
#8833 = CARTESIAN_POINT ( 'NONE',  ( 62.90077106633562209, -14.84248999999999974, 8.141649473166729933 ) ) ;
#8834 = CARTESIAN_POINT ( 'NONE',  ( 20.92131311655350245, -1.145359114192535888, -15.19233952661473097 ) ) ;
#8835 = CYLINDRICAL_SURFACE ( 'NONE', #317, 11.02160133116777452 ) ;
#8836 = ORIENTED_EDGE ( 'NONE', *, *, #16985, .F. ) ;
#8837 = CARTESIAN_POINT ( 'NONE',  ( 9.146678809762240903, 19.11784201969034314, -2.518986951451899436 ) ) ;
#8838 = VECTOR ( 'NONE', #2034, 1000.000000000000000 ) ;
#8839 = CARTESIAN_POINT ( 'NONE',  ( -1.351150467732365579, 3.961447500000001565, -27.17319717629097653 ) ) ;
#8840 = CARTESIAN_POINT ( 'NONE',  ( 11.51458866710784434, 21.99093949232998213, 2.562257468935384530 ) ) ;
#8841 = VERTEX_POINT ( 'NONE', #19542 ) ;
#8842 = EDGE_CURVE ( 'NONE', #15164, #21307, #12928, .T. ) ;
#8843 = ORIENTED_EDGE ( 'NONE', *, *, #17042, .F. ) ;
#8844 = CARTESIAN_POINT ( 'NONE',  ( 13.03574908598719517, 21.42208332277566285, 0.9446814558890389568 ) ) ;
#8845 = CARTESIAN_POINT ( 'NONE',  ( 9.288485439755762130, 12.58942835895980572, 6.591978047692478526 ) ) ;
#8846 = CARTESIAN_POINT ( 'NONE',  ( 6.327178061961348909, 11.65658372465740200, 2.461826360968837779 ) ) ;
#8847 = CARTESIAN_POINT ( 'NONE',  ( 5.606189282461859769, 16.04232475255113499, -1.387877448415188342 ) ) ;
#8848 = VECTOR ( 'NONE', #7727, 1000.000000000000114 ) ;
#8849 = VECTOR ( 'NONE', #8170, 1000.000000000000000 ) ;
#8850 = CIRCLE ( 'NONE', #14191, 3.175000000000001155 ) ;
#8851 = DIRECTION ( 'NONE',  ( -0.9987059298363656357, 0.000000000000000000, -0.05085730733808393328 ) ) ;
#8852 = CARTESIAN_POINT ( 'NONE',  ( 7.848665660996588578, 21.72673311005876329, 3.154536144953404175 ) ) ;
#8853 = CARTESIAN_POINT ( 'NONE',  ( 4.966346748821892199, 12.29804937889246119, 5.546774599257833671 ) ) ;
#8854 = CARTESIAN_POINT ( 'NONE',  ( 32.17043356788648367, 37.11476346399999926, -17.71146456218788146 ) ) ;
#8855 = CARTESIAN_POINT ( 'NONE',  ( 3.884858786145676035, 12.19654146317258103, 0.3546744299869324935 ) ) ;
#8856 = CARTESIAN_POINT ( 'NONE',  ( 1.388599495393930683, 18.36893808807919015, 9.176162539399413731 ) ) ;
#8857 = CARTESIAN_POINT ( 'NONE',  ( 38.60701496492545459, -1.983739999999999837, -26.94161103631838472 ) ) ;
#8858 = CARTESIAN_POINT ( 'NONE',  ( 5.598452204629278839, 20.83490078207852392, 3.741209306395075540 ) ) ;
#8859 = DIRECTION ( 'NONE',  ( -0.08420877549337302259, 0.000000000000000000, -0.9964481331860212121 ) ) ;
#8860 = CARTESIAN_POINT ( 'NONE',  ( -12.21686131739395798, -0.3962399999999990929, -1.090609736204202429 ) ) ;
#8861 = CARTESIAN_POINT ( 'NONE',  ( 19.80084360436371682, 0.3372488075446856692, -14.31343108369374484 ) ) ;
#8862 = AXIS2_PLACEMENT_3D ( 'NONE', #10262, #5176, #17129 ) ;
#8863 = CIRCLE ( 'NONE', #5328, 0.3962399999999997591 ) ;
#8864 = CARTESIAN_POINT ( 'NONE',  ( 32.55306802826559220, 34.52875999999999834, -17.37731658638881527 ) ) ;
#8865 = CARTESIAN_POINT ( 'NONE',  ( 11.25546319390698535, 17.89488212436745229, 7.371895500363925713 ) ) ;
#8866 = EDGE_CURVE ( 'NONE', #12465, #171, #4177, .T. ) ;
#8867 = DIRECTION ( 'NONE',  ( 0.000000000000000000, 1.000000000000000000, 0.000000000000000000 ) ) ;
#8868 = ADVANCED_FACE ( 'NONE', ( #21300 ), #7497, .F. ) ;
#8869 = CIRCLE ( 'NONE', #20521, 1.984375000000000000 ) ;
#8870 = CARTESIAN_POINT ( 'NONE',  ( 11.37527975260994850, 18.06908308185732537, -3.317263757504213206 ) ) ;
#8871 = CARTESIAN_POINT ( 'NONE',  ( 49.41235866845560309, 0.000000000000000000, -26.78690084448080100 ) ) ;
#8872 = EDGE_LOOP ( 'NONE', ( #10395, #3194, #6579, #4610 ) ) ;
#8873 = AXIS2_PLACEMENT_3D ( 'NONE', #19791, #20296, #11916 ) ;
#8874 = LINE ( 'NONE', #12313, #16979 ) ;
#8875 =( BOUNDED_CURVE ( )  B_SPLINE_CURVE ( 3, ( #16734, #8315, #21798, #6652 ),
 .UNSPECIFIED., .F., .F. ) 
 B_SPLINE_CURVE_WITH_KNOTS ( ( 4, 4 ),
 ( 2.992738460178339999, 3.006667970820978031 ),
 .UNSPECIFIED. ) 
 CURVE ( )  GEOMETRIC_REPRESENTATION_ITEM ( )  RATIONAL_B_SPLINE_CURVE ( ( 1.000000000000000000, 0.9999838307931325776, 0.9999838307931325776, 1.000000000000000000 ) ) 
 REPRESENTATION_ITEM ( '' )  );
#8876 = FACE_OUTER_BOUND ( 'NONE', #7739, .T. ) ;
#8877 = CLOSED_SHELL ( 'NONE', ( #20140, #7656, #12487, #17525, #9213, #6154, #2208, #18803, #19920, #14748, #1545, #2670, #13784, #18439, #9882, #8926, #13950 ) ) ;
#8878 = CIRCLE ( 'NONE', #9587, 2.182812499999999378 ) ;
#8879 = VECTOR ( 'NONE', #14968, 1000.000000000000000 ) ;
#8880 = ORIENTED_EDGE ( 'NONE', *, *, #1863, .F. ) ;
#8881 = CARTESIAN_POINT ( 'NONE',  ( 7.626149225290501654, 21.00148274865230036, 3.166616558793210245 ) ) ;
#8882 = CARTESIAN_POINT ( 'NONE',  ( 4.529126002162273679, 19.77844967572892898, 6.376247277523235724 ) ) ;
#8883 = CARTESIAN_POINT ( 'NONE',  ( 14.13422953375516045, 20.59196267482642284, 3.825818811277526876 ) ) ;
#8884 = CARTESIAN_POINT ( 'NONE',  ( 3.281879507946431573, 11.63542902183100125, 5.027702361350555371 ) ) ;
#8885 = CARTESIAN_POINT ( 'NONE',  ( 17.30373842852263877, -1.983739999999999393, -12.15706637069277107 ) ) ;
#8886 = VECTOR ( 'NONE', #6396, 1000.000000000000000 ) ;
#8887 =( GEOMETRIC_REPRESENTATION_CONTEXT ( 3 ) GLOBAL_UNCERTAINTY_ASSIGNED_CONTEXT ( ( #20948 ) ) GLOBAL_UNIT_ASSIGNED_CONTEXT ( ( #3435, #15069, #13961 ) ) REPRESENTATION_CONTEXT ( 'NONE', 'WORKASPACE' ) );
#8888 = CARTESIAN_POINT ( 'NONE',  ( 30.78626241496060700, 0.001587500000000546807, -2.552201779827368622 ) ) ;
#8889 = CARTESIAN_POINT ( 'NONE',  ( 19.58772840857323772, -1.669332001046654801, -14.30030513082031618 ) ) ;
#8890 = CARTESIAN_POINT ( 'NONE',  ( -3.845402119898529758, 26.98019749999999917, -31.39393985263922460 ) ) ;
#8891 = ORIENTED_EDGE ( 'NONE', *, *, #14396, .T. ) ;
#8892 = CARTESIAN_POINT ( 'NONE',  ( 9.492769369201601748, 16.63237982350910826, 8.085771285227329130 ) ) ;
#8893 = CARTESIAN_POINT ( 'NONE',  ( -51.84716326864270286, 38.25938500000000175, -70.46824097531958842 ) ) ;
#8894 = CIRCLE ( 'NONE', #430, 0.7950199999999982836 ) ;
#8895 = ORIENTED_EDGE ( 'NONE', *, *, #9400, .F. ) ;
#8896 = ADVANCED_FACE ( 'NONE', ( #9252 ), #16031, .F. ) ;
#8897 = CARTESIAN_POINT ( 'NONE',  ( 9.332239567752825593, 16.42172345158643765, -2.863492792668257625 ) ) ;
#8898 = FACE_OUTER_BOUND ( 'NONE', #10710, .T. ) ;
#8899 = FACE_OUTER_BOUND ( 'NONE', #6239, .T. ) ;
#8901 = CARTESIAN_POINT ( 'NONE',  ( 1.776692311943213420, -1.594802499999998124, -22.71488278333245603 ) ) ;
#8900 = CARTESIAN_POINT ( 'NONE',  ( 0.9717421347890942140, 18.89460405061472414, 9.004989399516528437 ) ) ;
#8902 = EDGE_LOOP ( 'NONE', ( #16017, #5040, #4435, #8380 ) ) ;
#8903 = CARTESIAN_POINT ( 'NONE',  ( 7.473138860522134941, 13.60421353648831300, 7.673710903342175982 ) ) ;
#8904 = VECTOR ( 'NONE', #18736, 1000.000000000000000 ) ;
#8905 = CYLINDRICAL_SURFACE ( 'NONE', #11252, 0.5079999999999996740 ) ;
#8906 = ORIENTED_EDGE ( 'NONE', *, *, #3020, .T. ) ;
#8907 = VECTOR ( 'NONE', #20620, 1000.000000000000227 ) ;
#8908 = DIRECTION ( 'NONE',  ( -0.9987059298363656357, 0.000000000000000000, -0.05085730733808393328 ) ) ;
#8909 = CARTESIAN_POINT ( 'NONE',  ( -7.545238043312568088, 34.12394749999999988, -33.79351368943453338 ) ) ;
#8910 = ORIENTED_EDGE ( 'NONE', *, *, #21706, .F. ) ;
#8911 = LINE ( 'NONE', #2399, #21631 ) ;
#8912 = AXIS2_PLACEMENT_3D ( 'NONE', #14987, #9754, #21473 ) ;
#8913 = DIRECTION ( 'NONE',  ( 0.2868778675745011220, 0.000000000000000000, 0.9579671649362033747 ) ) ;
#8914 = DIRECTION ( 'NONE',  ( 0.000000000000000000, 1.000000000000000000, 0.000000000000000000 ) ) ;
#8915 = AXIS2_PLACEMENT_3D ( 'NONE', #8382, #8492, #208 ) ;
#8916 = CARTESIAN_POINT ( 'NONE',  ( -0.8970842057359728061, 34.12394749999999988, -22.54358764576276286 ) ) ;
#8917 = CIRCLE ( 'NONE', #8570, 3.970019999999999438 ) ;
#8918 = VERTEX_POINT ( 'NONE', #4293 ) ;
#8919 = DIRECTION ( 'NONE',  ( 0.000000000000000000, 1.000000000000000000, 0.000000000000000000 ) ) ;
#8920 = FACE_OUTER_BOUND ( 'NONE', #13783, .T. ) ;
#8921 = DIRECTION ( 'NONE',  ( 0.000000000000000000, 1.000000000000000000, 0.000000000000000000 ) ) ;
#8923 = CARTESIAN_POINT ( 'NONE',  ( 13.63956567280660614, -6.673707092738088598, -15.35198154347669508 ) ) ;
#8922 = DIRECTION ( 'NONE',  ( 0.000000000000000000, 0.000000000000000000, -1.000000000000000000 ) ) ;
#8924 = ORIENTED_EDGE ( 'NONE', *, *, #21796, .T. ) ;
#8925 = ORIENTED_EDGE ( 'NONE', *, *, #14569, .F. ) ;
#8926 = ADVANCED_FACE ( 'NONE', ( #862, #21081 ), #960, .F. ) ;
#8927 = CARTESIAN_POINT ( 'NONE',  ( 13.04321057777464787, 16.70014932840772204, 6.526733902502721563 ) ) ;
#8929 = LINE ( 'NONE', #5497, #12084 ) ;
#8928 = CARTESIAN_POINT ( 'NONE',  ( 7.302229971812547404, 18.51489551114278953, 8.052680363647331419 ) ) ;
#8930 = VERTEX_POINT ( 'NONE', #6045 ) ;
#8932 = CARTESIAN_POINT ( 'NONE',  ( 14.54968198082151609, -8.672570558313584144, -15.03874522469199171 ) ) ;
#8931 = CARTESIAN_POINT ( 'NONE',  ( 5.354525716978236538, 12.51143086260616144, 7.194241134548868821 ) ) ;
#8933 = VECTOR ( 'NONE', #4425, 1000.000000000000114 ) ;
#8934 = ORIENTED_EDGE ( 'NONE', *, *, #21176, .T. ) ;
#8935 = EDGE_LOOP ( 'NONE', ( #8722, #18397, #14584, #14040 ) ) ;
#8936 = CARTESIAN_POINT ( 'NONE',  ( 7.442367890852062295, 14.90359003035201191, -1.906045328434554653 ) ) ;
#8937 = VERTEX_POINT ( 'NONE', #12816 ) ;
#8938 = EDGE_CURVE ( 'NONE', #4294, #2096, #7090, .T. ) ;
#8939 = DIRECTION ( 'NONE',  ( 0.000000000000000000, -1.000000000000000000, 0.000000000000000000 ) ) ;
#8940 = AXIS2_PLACEMENT_3D ( 'NONE', #4499, #4607, #12689 ) ;
#8941 = CARTESIAN_POINT ( 'NONE',  ( 38.20353551528305047, -6.675755166547726382, -4.900394175645134354 ) ) ;
#8942 = CARTESIAN_POINT ( 'NONE',  ( 59.89111109153450485, 0.000000000000000000, -22.14529389979288965 ) ) ;
#8943 = DIRECTION ( 'NONE',  ( -0.05085730733808459941, 0.000000000000000000, 0.9987059298363656357 ) ) ;
#8944 = CARTESIAN_POINT ( 'NONE',  ( 2.636384871323212753, 20.46330206851546052, 7.042598730623302217 ) ) ;
#8945 = PLANE ( 'NONE',  #13361 ) ;
#8946 = ORIENTED_EDGE ( 'NONE', *, *, #9301, .T. ) ;
#8947 = CARTESIAN_POINT ( 'NONE',  ( 7.320132777942092162, 12.26967076330688222, 5.547411630589742515 ) ) ;
#8948 = LINE ( 'NONE', #15726, #11709 ) ;
#8949 = VERTEX_POINT ( 'NONE', #18312 ) ;
#8950 = VERTEX_POINT ( 'NONE', #4932 ) ;
#8951 = EDGE_CURVE ( 'NONE', #18019, #12607, #14879, .T. ) ;
#8952 = CARTESIAN_POINT ( 'NONE',  ( 8.286930802166120102, 19.91511611422710359, 6.446135514764869789 ) ) ;
#8953 = AXIS2_PLACEMENT_3D ( 'NONE', #3617, #11802, #5479 ) ;
#8954 = EDGE_CURVE ( 'NONE', #13795, #15382, #10259, .T. ) ;
#8955 = EDGE_CURVE ( 'NONE', #2722, #10050, #21408, .T. ) ;
#8956 = LINE ( 'NONE', #12177, #15623 ) ;
#8957 = CARTESIAN_POINT ( 'NONE',  ( 11.96407914667388361, 10.46320835736658239, 0.6102883513782707547 ) ) ;
#8958 = ORIENTED_EDGE ( 'NONE', *, *, #6753, .F. ) ;
#8959 = EDGE_LOOP ( 'NONE', ( #2167, #3613 ) ) ;
#8960 = CARTESIAN_POINT ( 'NONE',  ( 24.71252020198295085, 23.75961143032650114, -0.7333271064221494884 ) ) ;
#8961 = CARTESIAN_POINT ( 'NONE',  ( 7.434653127054422050, 12.56819603257475748, -1.447669836965668644 ) ) ;
#8962 = CARTESIAN_POINT ( 'NONE',  ( 6.215497495051750754, 20.44527992609954126, 5.212841242474709702 ) ) ;
#8963 = CARTESIAN_POINT ( 'NONE',  ( 8.505511374756364873, -6.752907499999998286, -20.97439202360551747 ) ) ;
#8964 = CARTESIAN_POINT ( 'NONE',  ( 6.126552632935823972, 11.96686506477097645, 1.644263794841153370 ) ) ;
#8965 = PLANE ( 'NONE',  #1540 ) ;
#8966 = CARTESIAN_POINT ( 'NONE',  ( 11.59039627428740005, 17.69506805168922980, 7.363997034513484863 ) ) ;
#8967 = CIRCLE ( 'NONE', #21327, 3.970020000000000326 ) ;
#8968 = EDGE_CURVE ( 'NONE', #1968, #20661, #9578, .T. ) ;
#8969 = CARTESIAN_POINT ( 'NONE',  ( 39.58386072796550081, 38.88803500000000213, -4.490541772578183100 ) ) ;
#8970 = CARTESIAN_POINT ( 'NONE',  ( 1.621773686558225069, 14.62646646242487769, -0.4960749032165705508 ) ) ;
#8971 = CARTESIAN_POINT ( 'NONE',  ( 1.567395821070151074, 17.31328409496832066, 9.515441300692291549 ) ) ;
#8972 = DIRECTION ( 'NONE',  ( -0.9579671649362032637, 0.000000000000000000, 0.2868778675745010664 ) ) ;
#8973 = CARTESIAN_POINT ( 'NONE',  ( 6.053126112950039328, 12.01118930601124291, 1.445651676772871319 ) ) ;
#8974 = DIRECTION ( 'NONE',  ( 0.000000000000000000, 1.000000000000000000, 0.000000000000000000 ) ) ;
#8975 = CARTESIAN_POINT ( 'NONE',  ( 46.03750000000000142, -14.84248999999999974, -10.31874999999999964 ) ) ;
#8976 = CARTESIAN_POINT ( 'NONE',  ( 20.94353291967679453, -2.672331840313235674, -13.89923075121346230 ) ) ;
#8977 = AXIS2_PLACEMENT_3D ( 'NONE', #20711, #2481, #5567 ) ;
#8978 = DIRECTION ( 'NONE',  ( -0.9129422336036127072, 0.000000000000000000, 0.4080888115384278536 ) ) ;
#8979 = EDGE_CURVE ( 'NONE', #14819, #12179, #14704, .T. ) ;
#8980 = CARTESIAN_POINT ( 'NONE',  ( 10.50516453618270951, 10.67034598166200077, 3.014593022769773256 ) ) ;
#8981 = VERTEX_POINT ( 'NONE', #16562 ) ;
#8982 = CARTESIAN_POINT ( 'NONE',  ( 11.26949333533593922, -4.616615725918594038, -15.82154907933577448 ) ) ;
#8983 = CARTESIAN_POINT ( 'NONE',  ( 11.19867328698874687, 16.63172145237887278, -3.589918250282487122 ) ) ;
#8984 = DIRECTION ( 'NONE',  ( -0.2490110332224850231, 0.000000000000000000, 0.9685006480810791629 ) ) ;
#8985 = AXIS2_PLACEMENT_3D ( 'NONE', #13124, #8235, #19837 ) ;
#8986 = ORIENTED_EDGE ( 'NONE', *, *, #758, .T. ) ;
#8987 = DIRECTION ( 'NONE',  ( 1.000000000000000000, 0.000000000000000000, 0.000000000000000000 ) ) ;
#8988 = FILL_AREA_STYLE_COLOUR ( '', #19454 ) ;
#8989 = CARTESIAN_POINT ( 'NONE',  ( 5.060608184540046572, 20.55003013079386065, 2.242568649026101646 ) ) ;
#8990 = DIRECTION ( 'NONE',  ( 0.2490110332224846623, 0.000000000000000000, -0.9685006480810793850 ) ) ;
#8991 = CIRCLE ( 'NONE', #16437, 0.7950200000000003930 ) ;
#8992 = ORIENTED_EDGE ( 'NONE', *, *, #1932, .T. ) ;
#8993 = CARTESIAN_POINT ( 'NONE',  ( 8.715318583361199245, 19.62664610146546096, 6.014593122911379375 ) ) ;
#8994 = ADVANCED_FACE ( 'NONE', ( #16665 ), #11680, .F. ) ;
#8995 = CARTESIAN_POINT ( 'NONE',  ( 13.94935210066752163, 20.92845091260043944, 3.339972092365505407 ) ) ;
#8996 = CARTESIAN_POINT ( 'NONE',  ( 3.949281531805286072, 14.74976095948969679, 8.888991823293663330 ) ) ;
#8997 = EDGE_CURVE ( 'NONE', #3294, #6310, #4613, .T. ) ;
#8998 = CARTESIAN_POINT ( 'NONE',  ( 11.94677749553334323, 10.33025398667194139, 0.6609700684136409210 ) ) ;
#8999 = EDGE_CURVE ( 'NONE', #1735, #7286, #20784, .T. ) ;
#9000 = CARTESIAN_POINT ( 'NONE',  ( 19.80556909575297908, -1.573965866645507861, -15.31865534271369711 ) ) ;
#9001 = CARTESIAN_POINT ( 'NONE',  ( 16.92565045872677487, 0.9375092998980070202, -15.17115336936947934 ) ) ;
#9002 = CARTESIAN_POINT ( 'NONE',  ( -29.36874999999999858, 30.56064500000000095, -3.968750000000000000 ) ) ;
#9003 = EDGE_LOOP ( 'NONE', ( #4783, #11145, #10484, #7815 ) ) ;
#9004 = CARTESIAN_POINT ( 'NONE',  ( 11.12364941492027803, 17.00792697408808962, 6.778445003776157662 ) ) ;
#9005 = CARTESIAN_POINT ( 'NONE',  ( 11.48982677350561232, 15.66509967140728854, 7.652876522509257207 ) ) ;
#9006 = AXIS2_PLACEMENT_3D ( 'NONE', #17959, #6007, #17856 ) ;
#9007 = EDGE_LOOP ( 'NONE', ( #11475, #20386, #14705 ) ) ;
#9008 = CARTESIAN_POINT ( 'NONE',  ( 9.295090217099296837, 15.49936585922396937, -2.781353060168781255 ) ) ;
#9009 = CARTESIAN_POINT ( 'NONE',  ( 53.10651001381376091, -5.166360000000002728, -16.70269254552787075 ) ) ;
#9010 = CARTESIAN_POINT ( 'NONE',  ( -0.8970842057359728061, 25.39269750000000059, -22.54358764576276286 ) ) ;
#9012 = DIRECTION ( 'NONE',  ( -0.000000000000000000, 1.000000000000000000, 0.000000000000000000 ) ) ;
#9011 = CARTESIAN_POINT ( 'NONE',  ( 3.093622439059696472, 16.50247895544803711, 9.043415154008217272 ) ) ;
#9013 = ORIENTED_EDGE ( 'NONE', *, *, #544, .T. ) ;
#9014 = CARTESIAN_POINT ( 'NONE',  ( 7.090215797885481841, 11.68299152395092122, 5.835935845868474026 ) ) ;
#9015 = CARTESIAN_POINT ( 'NONE',  ( 1.854799496439154316, 13.08893749999999834, 3.211081754263136911 ) ) ;
#9016 = VERTEX_POINT ( 'NONE', #1394 ) ;
#9017 = LINE ( 'NONE', #17315, #13566 ) ;
#9018 = CARTESIAN_POINT ( 'NONE',  ( 14.81625953204187596, -7.424720918027729155, -15.06137846235305844 ) ) ;
#9019 = ORIENTED_EDGE ( 'NONE', *, *, #8788, .F. ) ;
#9020 = CARTESIAN_POINT ( 'NONE',  ( 30.41963056417667488, 0.000000000000000000, -8.653862521447852174 ) ) ;
#9021 = CARTESIAN_POINT ( 'NONE',  ( 2.109252989286876101, 17.81722186424291721, 0.3028858017987954843 ) ) ;
#9022 = AXIS2_PLACEMENT_3D ( 'NONE', #18067, #20025, #8096 ) ;
#9023 = EDGE_CURVE ( 'NONE', #3908, #6031, #8136, .T. ) ;
#9024 = CARTESIAN_POINT ( 'NONE',  ( 11.41261416030154408, 22.17023050789328309, 2.001960333732383024 ) ) ;
#9025 = CARTESIAN_POINT ( 'NONE',  ( -20.57102662672950544, 33.73373999999999739, 0.6462872510839711149 ) ) ;
#9026 = DIRECTION ( 'NONE',  ( 0.08420877549337300871, 0.000000000000000000, 0.9964481331860212121 ) ) ;
#9027 = EDGE_LOOP ( 'NONE', ( #1882, #14028, #12561, #19160 ) ) ;
#9028 = CARTESIAN_POINT ( 'NONE',  ( 13.67756757867809725, 12.29391749999999739, 2.571257636385987144 ) ) ;
#9029 = DIRECTION ( 'NONE',  ( -0.9564948366894091558, 0.05542109139015080621, 0.2864369564417710845 ) ) ;
#9030 = FACE_OUTER_BOUND ( 'NONE', #18319, .T. ) ;
#9031 = VERTEX_POINT ( 'NONE', #16457 ) ;
#9032 = EDGE_LOOP ( 'NONE', ( #20292, #5902, #15868, #4321 ) ) ;
#9034 = DIRECTION ( 'NONE',  ( -0.2490110332224850509, 0.000000000000000000, 0.9685006480810792739 ) ) ;
#9033 = CARTESIAN_POINT ( 'NONE',  ( 4.090788008712939572, 21.31629319454957994, 5.251805483008242348 ) ) ;
#9035 = VERTEX_POINT ( 'NONE', #18108 ) ;
#9037 = CARTESIAN_POINT ( 'NONE',  ( 14.20533558566156884, -7.867031480749381522, -15.79333615885272835 ) ) ;
#9036 = CARTESIAN_POINT ( 'NONE',  ( 5.279029129154737987, 12.19382779458062771, 6.839692948426927543 ) ) ;
#9038 = EDGE_LOOP ( 'NONE', ( #19638, #9836, #19493, #19851 ) ) ;
#9039 = ORIENTED_EDGE ( 'NONE', *, *, #21034, .T. ) ;
#9040 = ORIENTED_EDGE ( 'NONE', *, *, #15467, .T. ) ;
#9041 = CARTESIAN_POINT ( 'NONE',  ( 3.240852002830010292, 13.09810700923016036, 7.006825282356911266 ) ) ;
#9042 = ADVANCED_FACE ( 'NONE', ( #20172 ), #2965, .T. ) ;
#9043 = CARTESIAN_POINT ( 'NONE',  ( -2.607150795738780058, 0.000000000000000000, 8.731885000000000119 ) ) ;
#9044 = DIRECTION ( 'NONE',  ( 0.000000000000000000, -1.000000000000000000, -0.000000000000000000 ) ) ;
#9045 = CARTESIAN_POINT ( 'NONE',  ( 21.43124999999999858, 16.27314499999999953, 10.71562499999999929 ) ) ;
#9046 = CARTESIAN_POINT ( 'NONE',  ( 12.02474915109715603, -95.96551800000000298, -13.51434638588835391 ) ) ;
#9047 = CARTESIAN_POINT ( 'NONE',  ( 3.600293491139347157, 16.51615582718421393, 9.202227310041637409 ) ) ;
#9048 = VERTEX_POINT ( 'NONE', #8253 ) ;
#9049 = CARTESIAN_POINT ( 'NONE',  ( 5.230971163609982710, 12.02159401923784010, 5.278208563677478260 ) ) ;
#9050 = CARTESIAN_POINT ( 'NONE',  ( 11.81489480681374715, -4.423560566030090513, -15.68132100509055782 ) ) ;
#9051 = CARTESIAN_POINT ( 'NONE',  ( 13.15941616736590802, 22.07931810055205446, 2.007639991878180652 ) ) ;
#9052 = CARTESIAN_POINT ( 'NONE',  ( -1.000942312354703878, 9.129395000000000593, 10.71562499999999929 ) ) ;
#9053 = DIRECTION ( 'NONE',  ( -0.9129422336036122632, 0.000000000000000000, 0.4080888115384288528 ) ) ;
#9054 = ORIENTED_EDGE ( 'NONE', *, *, #6753, .T. ) ;
#9055 = ORIENTED_EDGE ( 'NONE', *, *, #16984, .T. ) ;
#9056 = CARTESIAN_POINT ( 'NONE',  ( 10.31787650444773341, 11.27323348914452161, 4.153725677044106668 ) ) ;
#9057 = AXIS2_PLACEMENT_3D ( 'NONE', #4370, #4806, #16211 ) ;
#9059 = CARTESIAN_POINT ( 'NONE',  ( 37.19264538843808765, -6.356984999999999886, -4.718486965773546871 ) ) ;
#9058 = DIRECTION ( 'NONE',  ( 0.2868778675745011220, 0.000000000000000000, 0.9579671649362034858 ) ) ;
#9060 = CARTESIAN_POINT ( 'NONE',  ( 11.97810099218075308, 10.45522238918808178, 0.6684068655140054105 ) ) ;
#9061 = ORIENTED_EDGE ( 'NONE', *, *, #10717, .F. ) ;
#9062 = ORIENTED_EDGE ( 'NONE', *, *, #16650, .T. ) ;
#9063 = CYLINDRICAL_SURFACE ( 'NONE', #12374, 0.7950199999999996159 ) ;
#9064 = CARTESIAN_POINT ( 'NONE',  ( 7.250640286420714453, 16.37904396954605701, -2.887332892799749917 ) ) ;
#9065 = CARTESIAN_POINT ( 'NONE',  ( 6.106529886068845947, 12.01118930601124291, 1.429659103004671250 ) ) ;
#9066 = DIRECTION ( 'NONE',  ( 0.000000000000000000, -1.000000000000000000, -0.000000000000000000 ) ) ;
#9067 = CARTESIAN_POINT ( 'NONE',  ( 5.819762523047388392, 17.94946781983131245, -1.138627438642019429 ) ) ;
#9068 = CARTESIAN_POINT ( 'NONE',  ( 7.098073765475375829, 12.80169766613603599, 6.043837936590163551 ) ) ;
#9069 = DIRECTION ( 'NONE',  ( -0.9987059298363656357, 0.000000000000000000, -0.05085730733808393328 ) ) ;
#9070 = ADVANCED_FACE ( 'NONE', ( #13144 ), #1089, .T. ) ;
#9071 = VECTOR ( 'NONE', #16062, 1000.000000000000114 ) ;
#9072 = CARTESIAN_POINT ( 'NONE',  ( 9.469108807279354778, 17.35598761042881577, -3.664943468583037767 ) ) ;
#9073 = EDGE_CURVE ( 'NONE', #19208, #15022, #3168, .T. ) ;
#9074 = CARTESIAN_POINT ( 'NONE',  ( 3.243422562972307688, 11.89954130989696246, 6.891751807687494846 ) ) ;
#9075 = CARTESIAN_POINT ( 'NONE',  ( 0.8494540250199152931, 20.05826837460356771, 7.883665465059968014 ) ) ;
#9076 = DIRECTION ( 'NONE',  ( 0.000000000000000000, 1.000000000000000000, 0.000000000000000000 ) ) ;
#9077 = CARTESIAN_POINT ( 'NONE',  ( 0.01944810670579354139, 14.29202264928412092, 1.254942201865596463 ) ) ;
#9078 = CARTESIAN_POINT ( 'NONE',  ( 32.17043356788648367, -1.983739999999999837, -17.71146456218788146 ) ) ;
#9079 = FACE_OUTER_BOUND ( 'NONE', #3940, .T. ) ;
#9080 = CARTESIAN_POINT ( 'NONE',  ( 14.91885465629891172, 2.197622263519783736, -15.77636844865548582 ) ) ;
#9081 = CARTESIAN_POINT ( 'NONE',  ( 151.3494547525804990, 22.62314500000000095, -45.56305690039940259 ) ) ;
#9082 = CARTESIAN_POINT ( 'NONE',  ( 11.44433539449762804, 15.04579128119321219, 7.441666735878229133 ) ) ;
#9083 = ORIENTED_EDGE ( 'NONE', *, *, #16650, .F. ) ;
#9084 = PLANE ( 'NONE',  #18059 ) ;
#9085 = CARTESIAN_POINT ( 'NONE',  ( 11.29905453907457868, 17.57833764777731744, -3.460908599073576397 ) ) ;
#9086 = VECTOR ( 'NONE', #442, 1000.000000000000227 ) ;
#9087 = CARTESIAN_POINT ( 'NONE',  ( 5.402704644578218307, 14.08031241623537255, -1.660995405501500155 ) ) ;
#9088 = LINE ( 'NONE', #17945, #21138 ) ;
#9089 = ORIENTED_EDGE ( 'NONE', *, *, #18579, .F. ) ;
#9090 = ITEM_DEFINED_TRANSFORMATION ( 'NONE', 'NONE', #19709,  #2234 ) ;
#9091 = EDGE_CURVE ( 'NONE', #9498, #7172, #19436, .T. ) ;
#9092 = CARTESIAN_POINT ( 'NONE',  ( -20.57102662672950544, 33.73373999999999739, 0.6462872510839712259 ) ) ;
#9093 = DIRECTION ( 'NONE',  ( -0.3482992169606098365, 0.9330960544336215357, -0.08955115110948595747 ) ) ;
#9094 = ORIENTED_EDGE ( 'NONE', *, *, #2742, .T. ) ;
#9095 = CARTESIAN_POINT ( 'NONE',  ( 11.12613972328005119, 16.27078869972546116, -3.689852400265816179 ) ) ;
#9096 = ADVANCED_FACE ( 'NONE', ( #3291 ), #1616, .T. ) ;
#9097 = CARTESIAN_POINT ( 'NONE',  ( 7.679475497374705917, 18.07321731131985842, -1.947026857138824063 ) ) ;
#9098 = CYLINDRICAL_SURFACE ( 'NONE', #16014, 1.587500000000002132 ) ;
#9099 = VECTOR ( 'NONE', #991, 1000.000000000000000 ) ;
#9100 = DIRECTION ( 'NONE',  ( 0.000000000000000000, 1.000000000000000000, 0.000000000000000000 ) ) ;
#9101 = ADVANCED_FACE ( 'NONE', ( #394 ), #17197, .T. ) ;
#9102 = CARTESIAN_POINT ( 'NONE',  ( 18.38685979067734166, 0.1402437363902317435, -14.71391125517748222 ) ) ;
#9103 = LINE ( 'NONE', #9002, #2122 ) ;
#9104 = ORIENTED_EDGE ( 'NONE', *, *, #11086, .T. ) ;
#9105 = AXIS2_PLACEMENT_3D ( 'NONE', #1368, #20037, #9999 ) ;
#9106 = CARTESIAN_POINT ( 'NONE',  ( 9.243180543658688464, 18.56570064461385527, 7.646858442508960962 ) ) ;
#9107 = CARTESIAN_POINT ( 'NONE',  ( 27.40895291499714403, 0.000000000000000000, -9.088367920799473865 ) ) ;
#9108 = VERTEX_POINT ( 'NONE', #11899 ) ;
#9109 = CARTESIAN_POINT ( 'NONE',  ( 10.68304280333123835, 11.74562633852015203, 3.840012745435023689 ) ) ;
#9110 = DIRECTION ( 'NONE',  ( 0.9685006480810792739, -0.000000000000000000, 0.2490110332224850509 ) ) ;
#9111 = CARTESIAN_POINT ( 'NONE',  ( 0.2158207035600169243, 20.08891550228490530, 6.180427975396654894 ) ) ;
#9113 = DIRECTION ( 'NONE',  ( 0.9579671649362032637, 0.000000000000000000, -0.2868778675745010664 ) ) ;
#9112 = CARTESIAN_POINT ( 'NONE',  ( -0.5255128162433173600, 15.65082615746288219, 0.5089085096668227726 ) ) ;
#9114 = ORIENTED_EDGE ( 'NONE', *, *, #19973, .T. ) ;
#9115 = CARTESIAN_POINT ( 'NONE',  ( 7.454305085027373323, 13.41251517923412706, 7.565232220981850553 ) ) ;
#9116 = EDGE_CURVE ( 'NONE', #17778, #21489, #15453, .T. ) ;
#9117 = CARTESIAN_POINT ( 'NONE',  ( 2.063750000000000195, 30.16440499999999858, 8.731249999999999289 ) ) ;
#9118 = ADVANCED_FACE ( 'NONE', ( #20612 ), #15681, .F. ) ;
#9119 = CARTESIAN_POINT ( 'NONE',  ( 38.23013820809905638, 109.3223030719999969, -14.22485453658974031 ) ) ;
#9120 = EDGE_CURVE ( 'NONE', #12008, #6512, #8850, .T. ) ;
#9121 = ORIENTED_EDGE ( 'NONE', *, *, #16069, .F. ) ;
#9122 = CARTESIAN_POINT ( 'NONE',  ( 19.35098353498187507, 0.3056836383201791962, -15.04733789981717251 ) ) ;
#9123 = CARTESIAN_POINT ( 'NONE',  ( 0.03927176397120358403, 15.80852762767634800, 0.8372861472476095246 ) ) ;
#9124 = PRODUCT ( 'Locking Pawl Compression Spring', 'Locking Pawl Compression Spring', '', ( #5335 ) ) ;
#9125 = CARTESIAN_POINT ( 'NONE',  ( 20.59926559563684378, -3.336837234538238217, -15.67345047278095471 ) ) ;
#9126 = EDGE_LOOP ( 'NONE', ( #11341, #14645 ) ) ;
#9127 = DIRECTION ( 'NONE',  ( -0.7421532822901579785, 0.000000000000000000, 0.6702301885068628895 ) ) ;
#9128 = PRODUCT_DEFINITION_FORMATION_WITH_SPECIFIED_SOURCE ( 'ANY', '', #4914, .NOT_KNOWN. ) ;
#9129 = DIRECTION ( 'NONE',  ( -0.6744690509234934073, -0.7360996206939023345, 0.05699866455150641442 ) ) ;
#9130 = DIRECTION ( 'NONE',  ( 0.000000000000000000, 1.000000000000000000, 0.000000000000000000 ) ) ;
#9131 = CIRCLE ( 'NONE', #21856, 3.968750000000000000 ) ;
#9132 = EDGE_LOOP ( 'NONE', ( #2736, #8544 ) ) ;
#9133 = LINE ( 'NONE', #18973, #21304 ) ;
#9134 = CARTESIAN_POINT ( 'NONE',  ( 0.02083138522551555155, 12.30439499999999953, 7.210477125664100484 ) ) ;
#9135 = EDGE_LOOP ( 'NONE', ( #6741, #19562, #3990, #17088 ) ) ;
#9136 = ORIENTED_EDGE ( 'NONE', *, *, #19670, .F. ) ;
#9138 = CARTESIAN_POINT ( 'NONE',  ( 2.063750000000000195, 8.334374999999999645, 8.731249999999999289 ) ) ;
#9137 = CARTESIAN_POINT ( 'NONE',  ( -0.2015346878679116771, 15.59640844431605267, -0.007168570956162228364 ) ) ;
#9139 = ORIENTED_EDGE ( 'NONE', *, *, #620, .F. ) ;
#9140 = CARTESIAN_POINT ( 'NONE',  ( 5.590944741272595664, 15.72999216326778260, 8.764459480800841362 ) ) ;
#9141 = EDGE_CURVE ( 'NONE', #10543, #3115, #3557, .T. ) ;
#9142 = VERTEX_POINT ( 'NONE', #18628 ) ;
#9143 = EDGE_CURVE ( 'NONE', #10936, #20661, #7148, .T. ) ;
#9144 = ORIENTED_EDGE ( 'NONE', *, *, #6855, .T. ) ;
#9145 = VECTOR ( 'NONE', #14119, 1000.000000000000000 ) ;
#9146 = ORIENTED_EDGE ( 'NONE', *, *, #14923, .T. ) ;
#9147 = CARTESIAN_POINT ( 'NONE',  ( 2.818771752949199350, 12.10965044584980888, 4.995725464678207217 ) ) ;
#9148 = CIRCLE ( 'NONE', #8456, 0.3962400000000008138 ) ;
#9149 = PLANE ( 'NONE',  #12437 ) ;
#9150 = AXIS2_PLACEMENT_3D ( 'NONE', #7317, #5651, #4109 ) ;
#9151 = CARTESIAN_POINT ( 'NONE',  ( 5.447351731530780228, 1.984375000000000000, 0.8930339070797439494 ) ) ;
#9152 = DIRECTION ( 'NONE',  ( -0.2490110332224836354, 0.000000000000000000, 0.9685006480810794960 ) ) ;
#9153 = CARTESIAN_POINT ( 'NONE',  ( 2.936231591482770131, 19.83055965519156416, 7.812606543334467801 ) ) ;
#9154 = ORIENTED_EDGE ( 'NONE', *, *, #5218, .T. ) ;
#9155 = CARTESIAN_POINT ( 'NONE',  ( 6.368383225667405334, 11.93222000202738187, 1.317153128801042072 ) ) ;
#9156 = DIRECTION ( 'NONE',  ( 0.000000000000000000, 0.000000000000000000, 1.000000000000000000 ) ) ;
#9157 = CARTESIAN_POINT ( 'NONE',  ( 54.11611804786240043, 0.000000000000000000, -30.58983753981140197 ) ) ;
#9158 = CARTESIAN_POINT ( 'NONE',  ( -22.33576604192310455, -0.3962399999999990929, 0.9319226134156143315 ) ) ;
#9159 = ORIENTED_EDGE ( 'NONE', *, *, #20990, .F. ) ;
#9160 = VERTEX_POINT ( 'NONE', #10128 ) ;
#9161 = CARTESIAN_POINT ( 'NONE',  ( 9.625378508224750718, 20.58315642183951866, -1.315007443808327237 ) ) ;
#9163 = CARTESIAN_POINT ( 'NONE',  ( 8.781357490942916399, -7.547927499999999235, -18.85455479843708559 ) ) ;
#9162 = LINE ( 'NONE', #4318, #17895 ) ;
#9164 = CARTESIAN_POINT ( 'NONE',  ( 13.38508960593052066, 14.68835664565479604, 6.944885673946169291 ) ) ;
#9165 = EDGE_LOOP ( 'NONE', ( #1511, #8167, #11920, #20502 ) ) ;
#9166 = ORIENTED_EDGE ( 'NONE', *, *, #16484, .T. ) ;
#9167 = EDGE_CURVE ( 'NONE', #18470, #18734, #6736, .T. ) ;
#9168 = CARTESIAN_POINT ( 'NONE',  ( 66.03921914090641110, 30.56064500000000095, -10.93409647675949969 ) ) ;
#9169 = CARTESIAN_POINT ( 'NONE',  ( 7.953648525153114157, 11.02408685177427117, 0.8496204234235359420 ) ) ;
#9170 = CARTESIAN_POINT ( 'NONE',  ( 4.040739369786842339, 20.53326216353070421, 5.052342526274332002 ) ) ;
#9171 = CYLINDRICAL_SURFACE ( 'NONE', #17957, 0.5079999999999984528 ) ;
#9172 = AXIS2_PLACEMENT_3D ( 'NONE', #18282, #13115, #18188 ) ;
#9173 = CIRCLE ( 'NONE', #11993, 25.00312500000000426 ) ;
#9174 = CARTESIAN_POINT ( 'NONE',  ( 8.750313129456580796, 19.14012259891230627, 6.327658032475317107 ) ) ;
#9175 = CARTESIAN_POINT ( 'NONE',  ( 7.321344744572315655, 14.84602651755674252, 7.391589468013401110 ) ) ;
#9176 = B_SPLINE_CURVE_WITH_KNOTS ( 'NONE', 3,
 ( #5448, #12210, #2250, #3804 ),
 .UNSPECIFIED., .F., .F.,
 ( 4, 4 ),
 ( 0.000000000000000000, 1.000000000000000000 ),
 .UNSPECIFIED. ) ;
#9177 = CARTESIAN_POINT ( 'NONE',  ( 1.940379840341371898, 20.36792767702591078, 5.166629419378853783 ) ) ;
#9178 = DIRECTION ( 'NONE',  ( -0.5733392046337749681, 0.8193181045417647912, 0.000000000000000000 ) ) ;
#9179 = DIRECTION ( 'NONE',  ( 0.000000000000000000, -1.000000000000000000, 0.000000000000000000 ) ) ;
#9180 = CARTESIAN_POINT ( 'NONE',  ( 12.87297671240983732, 10.82393886236346248, 2.518080570580241595 ) ) ;
#9181 = DIRECTION ( 'NONE',  ( -0.6702301885068652210, 0.000000000000000000, -0.7421532822901560911 ) ) ;
#9182 = CARTESIAN_POINT ( 'NONE',  ( 3.414760669001324800, 21.44980502101282127, 3.518543128841764567 ) ) ;
#9183 = CARTESIAN_POINT ( 'NONE',  ( 1.088531530542938830, 19.46978492123518478, 8.481480395730187638 ) ) ;
#9184 = CARTESIAN_POINT ( 'NONE',  ( 67.40134256979101224, 74.97070807199999365, -13.70358117861468017 ) ) ;
#9185 = CARTESIAN_POINT ( 'NONE',  ( 1.053492159257005678, 12.39630382929348151, 6.286052961942981909 ) ) ;
#9186 = DIRECTION ( 'NONE',  ( 0.7334850928793772429, 0.6768732144311025989, -0.06198604769976985562 ) ) ;
#9187 = CARTESIAN_POINT ( 'NONE',  ( -24.21104940531825633, -10.87373999999999974, -25.29232732678598339 ) ) ;
#9188 = CARTESIAN_POINT ( 'NONE',  ( 19.44826403579765284, 0.7519677144109497835, -14.42437082291665362 ) ) ;
#9189 = VERTEX_POINT ( 'NONE', #13790 ) ;
#9190 = CARTESIAN_POINT ( 'NONE',  ( -46.55710204590916135, -5.714364999999999029, -7.870588902259476605 ) ) ;
#9191 = CARTESIAN_POINT ( 'NONE',  ( 11.13272815207053412, 12.04177085653310719, 5.716067944331810757 ) ) ;
#9192 = ORIENTED_EDGE ( 'NONE', *, *, #5473, .T. ) ;
#9193 = CARTESIAN_POINT ( 'NONE',  ( 57.69402548289047417, -1.983739999999999837, -20.84562559047711261 ) ) ;
#9194 = ADVANCED_FACE ( 'NONE', ( #510 ), #15562, .F. ) ;
#9195 = CIRCLE ( 'NONE', #12032, 0.7950199999999993938 ) ;
#9196 = CARTESIAN_POINT ( 'NONE',  ( 5.452433434195132378, 13.50695901949029221, -1.362618185186349695 ) ) ;
#9197 = DIRECTION ( 'NONE',  ( 0.2868778675745011220, 0.000000000000000000, 0.9579671649362034858 ) ) ;
#9198 = AXIS2_PLACEMENT_3D ( 'NONE', #10563, #14020, #13680 ) ;
#9199 = ORIENTED_EDGE ( 'NONE', *, *, #10471, .T. ) ;
#9200 = CARTESIAN_POINT ( 'NONE',  ( -0.08564303786872971835, 20.23672349479678090, 5.121204619610163711 ) ) ;
#9201 = CARTESIAN_POINT ( 'NONE',  ( 6.119526778620084428, 20.42711211122828630, 5.032656639018053824 ) ) ;
#9202 = DIRECTION ( 'NONE',  ( 0.000000000000000000, -1.000000000000000000, 0.000000000000000000 ) ) ;
#9203 = CIRCLE ( 'NONE', #4269, 1.587499999999998579 ) ;
#9204 = CARTESIAN_POINT ( 'NONE',  ( 17.97854127242967337, -8.300061438778795875, -14.56394595263420477 ) ) ;
#9205 = ORIENTED_EDGE ( 'NONE', *, *, #15319, .T. ) ;
#9206 = CARTESIAN_POINT ( 'NONE',  ( 7.928377447478991868, 12.05201058041374118, 0.2304873749790961046 ) ) ;
#9207 = CARTESIAN_POINT ( 'NONE',  ( 4.411209516546746201, 19.98771269606189449, 6.079393835653899458 ) ) ;
#9208 = CARTESIAN_POINT ( 'NONE',  ( 11.37179424920164728, 18.10733791853621710, -3.426064086753738636 ) ) ;
#9209 = CARTESIAN_POINT ( 'NONE',  ( -12.58923395807689616, 5.421010862427522170E-16, -0.9319226134156151087 ) ) ;
#9210 = CIRCLE ( 'NONE', #399, 1.587499999999998579 ) ;
#9211 = AXIS2_PLACEMENT_3D ( 'NONE', #20251, #18711, #3370 ) ;
#9212 = DIRECTION ( 'NONE',  ( -0.3482992169606098365, 0.9330960544336215357, -0.08955115110948595747 ) ) ;
#9213 = ADVANCED_FACE ( 'NONE', ( #17309 ), #1720, .T. ) ;
#9214 = PRODUCT_DEFINITION_CONTEXT ( 'detailed design', #14579, 'design' ) ;
#9215 = DIRECTION ( 'NONE',  ( -0.1132953773954069598, 0.7241889112991808375, -0.6802312681817410667 ) ) ;
#9216 = ORIENTED_EDGE ( 'NONE', *, *, #19248, .T. ) ;
#9217 = CARTESIAN_POINT ( 'NONE',  ( 7.631829889725195493, 11.33951387506710162, -0.1018811746545836144 ) ) ;
#9218 = VECTOR ( 'NONE', #10970, 1000.000000000000227 ) ;
#9219 = DIRECTION ( 'NONE',  ( -0.9964481331860213231, 0.000000000000000000, 0.08420877549337311974 ) ) ;
#9220 = ORIENTED_EDGE ( 'NONE', *, *, #8664, .F. ) ;
#9221 = EDGE_CURVE ( 'NONE', #13909, #18557, #11796, .T. ) ;
#9222 = CARTESIAN_POINT ( 'NONE',  ( 10.46210129196975558, 11.44384454131881057, 2.868262577821945047 ) ) ;
#9223 = DIRECTION ( 'NONE',  ( 0.08420877549337300871, 0.000000000000000000, 0.9964481331860212121 ) ) ;
#9224 = CARTESIAN_POINT ( 'NONE',  ( 1.336750686926562848, 17.19894283162252790, 8.761756363425694971 ) ) ;
#9225 = EDGE_CURVE ( 'NONE', #11084, #171, #5311, .T. ) ;
#9226 = EDGE_CURVE ( 'NONE', #8349, #2994, #6581, .T. ) ;
#9228 = LINE ( 'NONE', #12791, #3573 ) ;
#9227 = CARTESIAN_POINT ( 'NONE',  ( 0.3464597092991406058, 19.87555530259703929, 7.760565032948996134 ) ) ;
#9229 = ORIENTED_EDGE ( 'NONE', *, *, #9813, .F. ) ;
#9230 = DIRECTION ( 'NONE',  ( 0.9790635044817342925, 0.000000000000000000, -0.2035550397114870569 ) ) ;
#9231 = CLOSED_SHELL ( 'NONE', ( #21826, #12597, #6852, #3182, #3585, #12612, #20119, #10996, #19671, #6949, #17071, #9096, #13483, #4136, #6703, #14723, #10981, #10004, #6081, #21521, #6706, #2999, #453, #16679, #868, #19211, #9352, #20616 ) ) ;
#9232 = CARTESIAN_POINT ( 'NONE',  ( 8.505511374756364873, 24.59767750000000319, -20.97439202360551747 ) ) ;
#9233 = VECTOR ( 'NONE', #14619, 1000.000000000000000 ) ;
#9234 = ORIENTED_EDGE ( 'NONE', *, *, #15634, .T. ) ;
#9235 = CARTESIAN_POINT ( 'NONE',  ( 19.38375428936542377, 0.2020908859931673240, -15.04237192290629110 ) ) ;
#9236 = CARTESIAN_POINT ( 'NONE',  ( 16.94501325483539844, 1.212346912392092024, -15.11607461051017331 ) ) ;
#9237 = ORIENTED_EDGE ( 'NONE', *, *, #18721, .T. ) ;
#9238 = CYLINDRICAL_SURFACE ( 'NONE', #20557, 19.05000000000000426 ) ;
#9239 = CARTESIAN_POINT ( 'NONE',  ( 59.55063415577301811, 0.000000000000000000, -22.52230776719629191 ) ) ;
#9240 = EDGE_CURVE ( 'NONE', #14134, #19333, #20480, .T. ) ;
#9241 = DIRECTION ( 'NONE',  ( -0.9964481331860213231, 0.000000000000000000, 0.08420877549337306422 ) ) ;
#9242 = VECTOR ( 'NONE', #4634, 1000.000000000000000 ) ;
#9243 = ORIENTED_EDGE ( 'NONE', *, *, #6025, .F. ) ;
#9244 = CARTESIAN_POINT ( 'NONE',  ( 11.75439013559175017, 128.5105379999999968, 4.331204221326972359 ) ) ;
#9245 = DIRECTION ( 'NONE',  ( 0.000000000000000000, 1.000000000000000000, 0.000000000000000000 ) ) ;
#9246 = ORIENTED_EDGE ( 'NONE', *, *, #16267, .F. ) ;
#9247 = ORIENTED_EDGE ( 'NONE', *, *, #5374, .F. ) ;
#9248 = DIRECTION ( 'NONE',  ( -0.6702301885068628895, 0.000000000000000000, -0.7421532822901579785 ) ) ;
#9249 = AXIS2_PLACEMENT_3D ( 'NONE', #18468, #17027, #8505 ) ;
#9250 = EDGE_CURVE ( 'NONE', #13702, #1, #17092, .T. ) ;
#9252 = FACE_OUTER_BOUND ( 'NONE', #21412, .T. ) ;
#9251 = CARTESIAN_POINT ( 'NONE',  ( 6.302627457059999827, 21.18238311700324417, 5.536129331643387275 ) ) ;
#9253 = ORIENTED_EDGE ( 'NONE', *, *, #5899, .T. ) ;
#9254 = CARTESIAN_POINT ( 'NONE',  ( 3.691539032982900093, 12.86983919638163520, -0.1392865449577171677 ) ) ;
#9255 = EDGE_LOOP ( 'NONE', ( #19620, #17222, #10590, #19665 ) ) ;
#9256 = ORIENTED_EDGE ( 'NONE', *, *, #13734, .F. ) ;
#9257 = CARTESIAN_POINT ( 'NONE',  ( 1.190075203671829840, 12.78130600077101064, 6.867397390420004299 ) ) ;
#9258 = VECTOR ( 'NONE', #5824, 1000.000000000000114 ) ;
#9259 = VERTEX_POINT ( 'NONE', #12127 ) ;
#9260 = AXIS2_PLACEMENT_3D ( 'NONE', #1357, #11213, #19933 ) ;
#9261 = AXIS2_PLACEMENT_3D ( 'NONE', #7728, #16151, #6067 ) ;
#9262 = DIRECTION ( 'NONE',  ( 0.000000000000000000, 1.000000000000000000, 0.000000000000000000 ) ) ;
#9263 = EDGE_CURVE ( 'NONE', #21520, #3969, #3719, .T. ) ;
#9264 = DIRECTION ( 'NONE',  ( -0.2868778675745011220, 0.000000000000000000, -0.9579671649362034858 ) ) ;
#9265 = DIRECTION ( 'NONE',  ( 0.000000000000000000, 1.000000000000000000, 0.000000000000000000 ) ) ;
#9266 = CYLINDRICAL_SURFACE ( 'NONE', #14680, 1.983740000000001391 ) ;
#9267 = CARTESIAN_POINT ( 'NONE',  ( 3.648412331247147034, 14.85656584819127879, 8.991936108934527994 ) ) ;
#9268 = EDGE_CURVE ( 'NONE', #17651, #21745, #12007, .T. ) ;
#9269 = ADVANCED_FACE ( 'NONE', ( #2494 ), #12719, .T. ) ;
#9270 = ORIENTED_EDGE ( 'NONE', *, *, #639, .F. ) ;
#9271 = CARTESIAN_POINT ( 'NONE',  ( 4.032829679376786380, 14.00947850804536721, -0.3008704057647156316 ) ) ;
#9272 = LINE ( 'NONE', #879, #5368 ) ;
#9273 = DIRECTION ( 'NONE',  ( -0.9685006480810792739, 0.000000000000000000, -0.2490110332224846346 ) ) ;
#9274 = CARTESIAN_POINT ( 'NONE',  ( 30.24348838687780727, -1.983739999999999837, -20.27293523655082552 ) ) ;
#9275 = AXIS2_PLACEMENT_3D ( 'NONE', #18544, #18440, #13476 ) ;
#9276 = ORIENTED_EDGE ( 'NONE', *, *, #2078, .F. ) ;
#9277 = ORIENTED_EDGE ( 'NONE', *, *, #18199, .T. ) ;
#9278 = CARTESIAN_POINT ( 'NONE',  ( 7.743276922147756203, 20.96234599748222038, 5.025255436566072653 ) ) ;
#9280 = CARTESIAN_POINT ( 'NONE',  ( 56.47666780297049627, 34.52875999999999834, 1.109116340531466127 ) ) ;
#9279 = CARTESIAN_POINT ( 'NONE',  ( 26.59062499999999929, 30.16440499999999858, 8.731249999999999289 ) ) ;
#9281 = CARTESIAN_POINT ( 'NONE',  ( 12.18403663738019738, 10.39853869505617112, 1.520800266583003379 ) ) ;
#9282 = ORIENTED_EDGE ( 'NONE', *, *, #18241, .F. ) ;
#9283 = EDGE_LOOP ( 'NONE', ( #14550, #21284, #6368, #16645 ) ) ;
#9284 = DIRECTION ( 'NONE',  ( 0.2227372614606430989, 0.000000000000000000, 0.9748785115885020280 ) ) ;
#9285 = CARTESIAN_POINT ( 'NONE',  ( 7.218832108077395837, 14.89085544374305670, -2.696453293844645938 ) ) ;
#9286 = VECTOR ( 'NONE', #19925, 1000.000000000000000 ) ;
#9287 = CARTESIAN_POINT ( 'NONE',  ( 1.886475874931245800, 14.88386107855003360, 0.2258545542662658556 ) ) ;
#9288 = LINE ( 'NONE', #5531, #284 ) ;
#9289 = CARTESIAN_POINT ( 'NONE',  ( 6.833200748973188965, 20.60529512528366780, 1.326882497385993620 ) ) ;
#9290 = CARTESIAN_POINT ( 'NONE',  ( 7.205660636103451644, 13.38211048488514088, 6.599037780638883355 ) ) ;
#9291 = DIRECTION ( 'NONE',  ( 0.2868778675745011220, 0.000000000000000000, 0.9579671649362034858 ) ) ;
#9292 = CIRCLE ( 'NONE', #21655, 0.3962400000000008138 ) ;
#9293 = DIRECTION ( 'NONE',  ( 0.8609107660235850723, 0.000000000000000000, -0.5087559856598092844 ) ) ;
#9294 = CARTESIAN_POINT ( 'NONE',  ( 11.04974211190474342, 19.58043239906450239, 6.708260239347588971 ) ) ;
#9295 = ADVANCED_BREP_SHAPE_REPRESENTATION ( '', ( #6635, #2234 ), #16895 ) ;
#9296 = CARTESIAN_POINT ( 'NONE',  ( 34.72145145287101542, 0.000000000000000000, 0.5851394578805096947 ) ) ;
#9297 = CARTESIAN_POINT ( 'NONE',  ( 49.41195815393805901, 34.52875999999999834, -1.411525001868561224 ) ) ;
#9298 = LINE ( 'NONE', #9510, #21526 ) ;
#9299 = CARTESIAN_POINT ( 'NONE',  ( 3.893743123751922663, 19.12659651351990320, -0.8000309555518917426 ) ) ;
#9300 = CARTESIAN_POINT ( 'NONE',  ( 1.039725201830166368, 11.58047422083137157, 6.064744957957070248 ) ) ;
#9301 = EDGE_CURVE ( 'NONE', #18266, #10543, #12339, .T. ) ;
#9302 = CARTESIAN_POINT ( 'NONE',  ( 39.37900608539015224, 37.69740999999999786, -4.303192893338801284 ) ) ;
#9303 = CARTESIAN_POINT ( 'NONE',  ( 4.897223231123858156, 12.10224027996176233, 5.344960981349180962 ) ) ;
#9304 = CARTESIAN_POINT ( 'NONE',  ( 1.954387715434429795, 23.81077936178774834, 10.71562499999999929 ) ) ;
#9305 = DIRECTION ( 'NONE',  ( 0.9579671649362033747, 0.000000000000000000, -0.2868778675745011220 ) ) ;
#9306 = ORIENTED_EDGE ( 'NONE', *, *, #21801, .F. ) ;
#9307 = CARTESIAN_POINT ( 'NONE',  ( 30.25543876212147509, -1.983739999999999837, -19.39939755251907272 ) ) ;
#9308 = CARTESIAN_POINT ( 'NONE',  ( 9.536567547932234490, 11.50748222034787105, -1.063888143023027588 ) ) ;
#9309 = ORIENTED_EDGE ( 'NONE', *, *, #4072, .F. ) ;
#9310 = VECTOR ( 'NONE', #2562, 1000.000000000000000 ) ;
#9311 = CARTESIAN_POINT ( 'NONE',  ( 29.64606458365116737, 36.49567249999999774, -15.53894806404596096 ) ) ;
#9312 = CARTESIAN_POINT ( 'NONE',  ( 5.401778888224800568, 16.44581222338524640, -2.160592110064928129 ) ) ;
#9313 = PLANE ( 'NONE',  #18662 ) ;
#9314 = ORIENTED_EDGE ( 'NONE', *, *, #11413, .T. ) ;
#9315 = CONTEXT_DEPENDENT_SHAPE_REPRESENTATION ( #6628, #15541 ) ;
#9316 = PLANE ( 'NONE',  #12772 ) ;
#9317 = CARTESIAN_POINT ( 'NONE',  ( 5.597516759145264587, 20.74156677563692597, 3.659026675076807678 ) ) ;
#9318 = APPLICATION_CONTEXT ( 'automotive_design' ) ;
#9319 = CARTESIAN_POINT ( 'NONE',  ( 32.17043356788648367, 0.000000000000000000, -17.71146456218788146 ) ) ;
#9320 = AXIS2_PLACEMENT_3D ( 'NONE', #19995, #16708, #12048 ) ;
#9321 = ORIENTED_EDGE ( 'NONE', *, *, #10902, .T. ) ;
#9322 = CARTESIAN_POINT ( 'NONE',  ( 10.60244234216251691, 11.17647817907412211, 2.092258798280409948 ) ) ;
#9323 = CARTESIAN_POINT ( 'NONE',  ( 5.243231333258746574, 17.19721735590602663, 7.955804737421353856 ) ) ;
#9324 = CIRCLE ( 'NONE', #18855, 0.7950200000000000600 ) ;
#9325 = CARTESIAN_POINT ( 'NONE',  ( 11.63500593880946177, 11.69841282151974227, -0.9689828243709948108 ) ) ;
#9326 = DIRECTION ( 'NONE',  ( 1.000000000000000000, 0.000000000000000000, 0.000000000000000000 ) ) ;
#9327 = ADVANCED_FACE ( 'NONE', ( #14129 ), #17868, .T. ) ;
#9328 = CARTESIAN_POINT ( 'NONE',  ( -23.01875000000000071, 30.56064500000000095, -10.31874999999999964 ) ) ;
#9329 = CARTESIAN_POINT ( 'NONE',  ( 12.11879977990919421, 12.29391749999999739, 0.1373704394269426865 ) ) ;
#9330 = CARTESIAN_POINT ( 'NONE',  ( 4.591792411387702444, 20.55650562689407579, 6.636581573250831312 ) ) ;
#9331 = CARTESIAN_POINT ( 'NONE',  ( -46.55773479047372376, -10.87373999999999974, -7.870535429687039120 ) ) ;
#9332 = ORIENTED_EDGE ( 'NONE', *, *, #16549, .F. ) ;
#9333 = AXIS2_PLACEMENT_3D ( 'NONE', #3584, #3376, #5129 ) ;
#9334 = CYLINDRICAL_SURFACE ( 'NONE', #4223, 0.5080000000000022276 ) ;
#9335 = EDGE_LOOP ( 'NONE', ( #20889, #505, #5035, #14593 ) ) ;
#9336 = CARTESIAN_POINT ( 'NONE',  ( 1.096763541954664856, 18.37323406418106586, 8.312844033778342023 ) ) ;
#9338 = CARTESIAN_POINT ( 'NONE',  ( 32.52436584422698473, 34.52875999999999834, 1.884807767196291284 ) ) ;
#9337 = CARTESIAN_POINT ( 'NONE',  ( 1.944119829274491229, 19.53481664226216452, 0.8650063851298049888 ) ) ;
#9339 = VERTEX_POINT ( 'NONE', #4155 ) ;
#9340 =( LENGTH_UNIT ( ) NAMED_UNIT ( * ) SI_UNIT ( .MILLI., .METRE. ) );
#9341 = AXIS2_PLACEMENT_3D ( 'NONE', #2426, #4191, #17242 ) ;
#9342 = DIRECTION ( 'NONE',  ( 0.000000000000000000, 1.000000000000000000, 0.000000000000000000 ) ) ;
#9343 = DIRECTION ( 'NONE',  ( -0.2672484743474505819, 0.000000000000000000, -0.9636276526537416176 ) ) ;
#9344 = ORIENTED_EDGE ( 'NONE', *, *, #20842, .T. ) ;
#9345 = CARTESIAN_POINT ( 'NONE',  ( -19.99570496368815142, -9.590920198756240467, -10.11526441440630286 ) ) ;
#9346 = CARTESIAN_POINT ( 'NONE',  ( 0.3678923928972068214, 18.28356801376448360, 1.246736171314209773 ) ) ;
#9347 = CARTESIAN_POINT ( 'NONE',  ( 17.43388704644383580, -7.135208455246296211, -14.50876463681930773 ) ) ;
#9348 = EDGE_LOOP ( 'NONE', ( #1072, #15034 ) ) ;
#9349 = DIRECTION ( 'NONE',  ( 0.000000000000000000, -1.000000000000000000, -0.000000000000000000 ) ) ;
#9350 = CARTESIAN_POINT ( 'NONE',  ( 1.928043380615611868, 16.41701505613207956, 0.06728629053293294637 ) ) ;
#9351 = CARTESIAN_POINT ( 'NONE',  ( 9.558161459289578943, 19.33115936737788232, -3.006980407988670390 ) ) ;
#9352 = ADVANCED_FACE ( 'NONE', ( #12570 ), #15896, .T. ) ;
#9353 = EDGE_CURVE ( 'NONE', #6731, #13482, #9228, .T. ) ;
#9354 = AXIS2_PLACEMENT_3D ( 'NONE', #19870, #8044, #16145 ) ;
#9355 = LINE ( 'NONE', #16122, #15460 ) ;
#9356 = ORIENTED_EDGE ( 'NONE', *, *, #16700, .F. ) ;
#9357 = CARTESIAN_POINT ( 'NONE',  ( 37.51913901087312553, -1.983739999999999837, -14.58057485080488114 ) ) ;
#9359 = DIRECTION ( 'NONE',  ( -0.4857267349359799535, 0.000000000000000000, 0.8741107132214044340 ) ) ;
#9358 = DIRECTION ( 'NONE',  ( -0.2064631973582987667, 0.000000000000000000, 0.9784543669157944601 ) ) ;
#9360 = EDGE_LOOP ( 'NONE', ( #12841, #16340, #15120, #6399 ) ) ;
#9361 = ORIENTED_EDGE ( 'NONE', *, *, #10075, .T. ) ;
#9362 = CARTESIAN_POINT ( 'NONE',  ( -14.99341658050716930, 36.73131074634049753, -10.07873794320098426 ) ) ;
#9364 = DIRECTION ( 'NONE',  ( 0.000000000000000000, 1.000000000000000000, 0.000000000000000000 ) ) ;
#9363 = CARTESIAN_POINT ( 'NONE',  ( 7.150949527180841869, 11.65893940570930276, 6.001705760337040729 ) ) ;
#9365 = ORIENTED_EDGE ( 'NONE', *, *, #8537, .T. ) ;
#9366 = CARTESIAN_POINT ( 'NONE',  ( 3.626612422794881052, 17.28006496868525232, -1.351333894438823569 ) ) ;
#9367 = EDGE_LOOP ( 'NONE', ( #21293, #19100, #4094, #8818 ) ) ;
#9368 = ORIENTED_EDGE ( 'NONE', *, *, #15943, .T. ) ;
#9369 = EDGE_CURVE ( 'NONE', #18111, #1622, #722, .T. ) ;
#9370 = VECTOR ( 'NONE', #11317, 1000.000000000000000 ) ;
#9371 = VERTEX_POINT ( 'NONE', #19514 ) ;
#9372 = CARTESIAN_POINT ( 'NONE',  ( 3.126795315295423983, 12.66988178275929222, 6.437474586529948084 ) ) ;
#9373 = EDGE_CURVE ( 'NONE', #15989, #3518, #16219, .T. ) ;
#9374 = FACE_OUTER_BOUND ( 'NONE', #3281, .T. ) ;
#9375 = LINE ( 'NONE', #17798, #5798 ) ;
#9376 = FACE_OUTER_BOUND ( 'NONE', #941, .T. ) ;
#9377 = CARTESIAN_POINT ( 'NONE',  ( 24.26606285357373594, 3.565842500000000914, -16.92219937337620195 ) ) ;
#9378 = CARTESIAN_POINT ( 'NONE',  ( 3.632498785534259866, 14.40071795978559699, 8.832255087646766256 ) ) ;
#9379 = ORIENTED_EDGE ( 'NONE', *, *, #1244, .F. ) ;
#9380 = CARTESIAN_POINT ( 'NONE',  ( 11.11006317807338561, -14.84248999999999974, 0.5252656612939419212 ) ) ;
#9381 = CARTESIAN_POINT ( 'NONE',  ( 54.78059207134182884, -6.356984999999999886, -16.96151288338074181 ) ) ;
#9382 = CARTESIAN_POINT ( 'NONE',  ( 13.11799571124250363, 13.08957250000000094, -19.78847697788343396 ) ) ;
#9383 = FACE_OUTER_BOUND ( 'NONE', #2870, .T. ) ;
#9384 = DIRECTION ( 'NONE',  ( 0.000000000000000000, 1.000000000000000000, 0.000000000000000000 ) ) ;
#9385 = ADVANCED_FACE ( 'NONE', ( #5700 ), #16008, .T. ) ;
#9386 = EDGE_LOOP ( 'NONE', ( #15707, #21873, #9603, #5985 ) ) ;
#9387 = VERTEX_POINT ( 'NONE', #17432 ) ;
#9388 = CARTESIAN_POINT ( 'NONE',  ( 7.527094280029700712, 11.97223945099518083, 0.3035030689026688155 ) ) ;
#9390 = CARTESIAN_POINT ( 'NONE',  ( 29.64606458365116737, -3.966527499999997097, -15.53894806404596096 ) ) ;
#9389 = DIRECTION ( 'NONE',  ( 0.9790635044817341814, 0.000000000000000000, -0.2035550397114870014 ) ) ;
#9391 = CARTESIAN_POINT ( 'NONE',  ( 13.38623696279685760, 14.73335078723855673, 6.957530059424012592 ) ) ;
#9392 = VERTEX_POINT ( 'NONE', #4049 ) ;
#9393 = VERTEX_POINT ( 'NONE', #837 ) ;
#9394 = FACE_OUTER_BOUND ( 'NONE', #1560, .T. ) ;
#9395 = CARTESIAN_POINT ( 'NONE',  ( 7.352509731926520686, 13.08366748006759650, -1.852861239733443410 ) ) ;
#9396 = CARTESIAN_POINT ( 'NONE',  ( 55.56250000000000000, 0.000000000000000000, -10.31874999999999964 ) ) ;
#9397 = EDGE_CURVE ( 'NONE', #4458, #6182, #11116, .T. ) ;
#9398 = CARTESIAN_POINT ( 'NONE',  ( 7.902835724841917653, 20.71418818157466646, 4.167812925585346662 ) ) ;
#9399 = EDGE_CURVE ( 'NONE', #19416, #1021, #1046, .T. ) ;
#9400 = EDGE_CURVE ( 'NONE', #9259, #20548, #12046, .T. ) ;
#9401 = CARTESIAN_POINT ( 'NONE',  ( 2.675095758391589751, 19.49110477356257576, 7.034375472487891301 ) ) ;
#9402 = CARTESIAN_POINT ( 'NONE',  ( 61.04701390398659555, -1.983739999999999837, -15.15157976445104993 ) ) ;
#9403 = DIRECTION ( 'NONE',  ( 0.000000000000000000, 1.000000000000000000, 0.000000000000000000 ) ) ;
#9404 = CARTESIAN_POINT ( 'NONE',  ( 12.76954518747143119, 10.51393144722840134, 2.621729904346445483 ) ) ;
#9405 = CARTESIAN_POINT ( 'NONE',  ( 13.44218100725569265, 22.16307759405859557, 1.935254454476087238 ) ) ;
#9406 = CARTESIAN_POINT ( 'NONE',  ( 49.13030338002142372, 32.54502000000000095, -2.154981381712871791 ) ) ;
#9407 = CARTESIAN_POINT ( 'NONE',  ( 5.340688094622302096, 12.35012481907357973, 7.188016169931777277 ) ) ;
#9408 = CARTESIAN_POINT ( 'NONE',  ( 0.9906448663280645883, 11.53243573101070218, 5.849629943059694526 ) ) ;
#9409 = CIRCLE ( 'NONE', #16827, 5.158739999999999881 ) ;
#9410 = CARTESIAN_POINT ( 'NONE',  ( 39.18461504901784309, 37.69700956874092412, -4.105368993849036308 ) ) ;
#9411 = CARTESIAN_POINT ( 'NONE',  ( 2.193444281137359564, 17.94014877828372079, 0.2300559325516845777 ) ) ;
#9412 = CARTESIAN_POINT ( 'NONE',  ( 61.02111788801703085, 32.54502000000000095, -5.406220493519755088 ) ) ;
#9413 = CARTESIAN_POINT ( 'NONE',  ( -29.36874999999999858, 1.984375000000000000, -13.26881841860929967 ) ) ;
#9414 = CARTESIAN_POINT ( 'NONE',  ( 11.67127651341588113, -6.514806905098483369, -15.79013620009136076 ) ) ;
#9415 = ORIENTED_EDGE ( 'NONE', *, *, #14997, .T. ) ;
#9416 = CARTESIAN_POINT ( 'NONE',  ( 29.64606458365116737, 30.55334249999999940, -15.53894806404596096 ) ) ;
#9417 = CARTESIAN_POINT ( 'NONE',  ( 11.44293608409318708, 15.29742052837710276, 7.486644574264715857 ) ) ;
#9418 = EDGE_LOOP ( 'NONE', ( #12375, #13618, #13059, #17624 ) ) ;
#9419 = DIRECTION ( 'NONE',  ( 0.000000000000000000, 1.000000000000000000, 0.000000000000000000 ) ) ;
#9420 = CARTESIAN_POINT ( 'NONE',  ( 5.389318750439047179, 16.20232685991933863, -2.152549537583109629 ) ) ;
#9421 = DIRECTION ( 'NONE',  ( -0.7334850928793772429, -0.6768732144311025989, 0.06198604769976985562 ) ) ;
#9422 = CARTESIAN_POINT ( 'NONE',  ( 0.7815218943751861547, 12.12637795047220202, 4.853680457913782220 ) ) ;
#9423 = ORIENTED_EDGE ( 'NONE', *, *, #8006, .T. ) ;
#9424 = PRESENTATION_STYLE_ASSIGNMENT (( #6107 ) ) ;
#9425 = CARTESIAN_POINT ( 'NONE',  ( 5.239375586970837162, 20.67732964299643683, 2.712271571789475644 ) ) ;
#9426 = ADVANCED_FACE ( 'NONE', ( #19183 ), #14241, .F. ) ;
#9427 = DIRECTION ( 'NONE',  ( 0.000000000000000000, 1.000000000000000000, 0.000000000000000000 ) ) ;
#9428 = CARTESIAN_POINT ( 'NONE',  ( 52.65345379380355695, 40.07865999999999929, -16.29354262597941982 ) ) ;
#9429 = CARTESIAN_POINT ( 'NONE',  ( 7.023078859562801313, 11.74208123617664157, 4.211509649359884477 ) ) ;
#9430 = DIRECTION ( 'NONE',  ( 0.000000000000000000, 0.000000000000000000, -1.000000000000000000 ) ) ;
#9431 = CARTESIAN_POINT ( 'NONE',  ( 3.903910055091213582, 16.51832937791753864, 9.132019056122507195 ) ) ;
#9432 = LINE ( 'NONE', #21149, #16024 ) ;
#9433 = DIRECTION ( 'NONE',  ( -0.6287118719681975554, 0.000000000000000000, -0.7776383362760898033 ) ) ;
#9434 = LINE ( 'NONE', #18866, #11843 ) ;
#9435 = CARTESIAN_POINT ( 'NONE',  ( -0.1849527688498912581, 20.63369000000000142, 5.150944030050081501 ) ) ;
#9436 = DIRECTION ( 'NONE',  ( -0.9987059298363656357, -0.000000000000000000, -0.05085730733808393328 ) ) ;
#9437 = AXIS2_PLACEMENT_3D ( 'NONE', #5160, #17212, #7164 ) ;
#9438 = EDGE_LOOP ( 'NONE', ( #12054, #21067, #6350, #5614 ) ) ;
#9439 = CARTESIAN_POINT ( 'NONE',  ( 50.29383871662588490, 0.000000000000000000, -28.02957329025317179 ) ) ;
#9440 = DIRECTION ( 'NONE',  ( -0.000000000000000000, -1.000000000000000000, 0.000000000000000000 ) ) ;
#9441 = EDGE_LOOP ( 'NONE', ( #15094, #4916, #12608, #11004 ) ) ;
#9442 = CARTESIAN_POINT ( 'NONE',  ( 9.965102658262930291, 19.76523925788982083, -1.574950225675940452 ) ) ;
#9443 = CARTESIAN_POINT ( 'NONE',  ( 3.360635606688116894, -3.968114999999999615, -20.45316710734507026 ) ) ;
#9444 = CARTESIAN_POINT ( 'NONE',  ( 1.472840618554822401, 15.71206864735696662, 8.805158946288562660 ) ) ;
#9445 = CARTESIAN_POINT ( 'NONE',  ( 20.24903775639316805, -5.937233424764036371, -13.47572151283328878 ) ) ;
#9447 = DIRECTION ( 'NONE',  ( -0.000000000000000000, -1.000000000000000000, 0.000000000000000000 ) ) ;
#9446 = CARTESIAN_POINT ( 'NONE',  ( 6.421918896133771426, 11.00346980177178224, 4.321624500989655004 ) ) ;
#9448 = ORIENTED_EDGE ( 'NONE', *, *, #1563, .F. ) ;
#9449 = FACE_OUTER_BOUND ( 'NONE', #8139, .T. ) ;
#9450 = EDGE_CURVE ( 'NONE', #4315, #12574, #19803, .T. ) ;
#9451 = CARTESIAN_POINT ( 'NONE',  ( 39.07267844585335581, -7.547610000000000596, -3.819438423585947540 ) ) ;
#9452 = ORIENTED_EDGE ( 'NONE', *, *, #17264, .T. ) ;
#9453 = CARTESIAN_POINT ( 'NONE',  ( 20.20304770538988137, -1.338751018026005379, -14.76265918450644854 ) ) ;
#9454 = CARTESIAN_POINT ( 'NONE',  ( 0.1865804364509018876, 17.36630291547838922, 0.9075020708449259565 ) ) ;
#9455 = VECTOR ( 'NONE', #20653, 1000.000000000000114 ) ;
#9456 = VERTEX_POINT ( 'NONE', #12672 ) ;
#9457 = CARTESIAN_POINT ( 'NONE',  ( 10.66833303431421065, 11.64719608603622270, 3.888054322948657493 ) ) ;
#9458 = CARTESIAN_POINT ( 'NONE',  ( 2.593946987045366637, 19.51451841538450438, 1.385786389991116030 ) ) ;
#9459 = CARTESIAN_POINT ( 'NONE',  ( 20.88124149777159388, -1.145906272312793517, -15.04208939847202409 ) ) ;
#9460 = CARTESIAN_POINT ( 'NONE',  ( 7.833861672054659664, 20.10324751469710236, -1.664036087720620172 ) ) ;
#9461 = CARTESIAN_POINT ( 'NONE',  ( 46.03750000000000142, 42.06303499999999929, -10.31874999999999964 ) ) ;
#9462 = VERTEX_POINT ( 'NONE', #19394 ) ;
#9463 = DIRECTION ( 'NONE',  ( 0.7421532822901579785, 0.000000000000000000, -0.6702301885068630005 ) ) ;
#9465 = DIRECTION ( 'NONE',  ( 0.000000000000000000, 1.000000000000000000, 0.000000000000000000 ) ) ;
#9464 = DIRECTION ( 'NONE',  ( 0.2490110332224850509, 0.000000000000000000, -0.9685006480810792739 ) ) ;
#9466 = VERTEX_POINT ( 'NONE', #11003 ) ;
#9467 = ORIENTED_EDGE ( 'NONE', *, *, #2472, .F. ) ;
#9468 = VECTOR ( 'NONE', #21792, 1000.000000000000000 ) ;
#9469 = DIRECTION ( 'NONE',  ( 0.2868778675745010664, 0.000000000000000000, 0.9579671649362032637 ) ) ;
#9471 = DIRECTION ( 'NONE',  ( 1.000000000000000000, 0.000000000000000000, 0.000000000000000000 ) ) ;
#9470 = CARTESIAN_POINT ( 'NONE',  ( 5.885296502875437596, 11.58475123937168050, 0.5917220264446930722 ) ) ;
#9472 = EDGE_LOOP ( 'NONE', ( #7251, #8032, #13260, #9763 ) ) ;
#9473 = CARTESIAN_POINT ( 'NONE',  ( 3.633444216715743913, 13.25045984076455774, -0.4357252384333677453 ) ) ;
#9474 = ORIENTED_EDGE ( 'NONE', *, *, #19924, .T. ) ;
#9475 = ADVANCED_FACE ( 'NONE', ( #17762 ), #20958, .F. ) ;
#9476 = ORIENTED_EDGE ( 'NONE', *, *, #17962, .T. ) ;
#9477 = AXIS2_PLACEMENT_3D ( 'NONE', #8010, #6786, #19833 ) ;
#9478 = ORIENTED_EDGE ( 'NONE', *, *, #13978, .T. ) ;
#9479 = AXIS2_PLACEMENT_3D ( 'NONE', #12796, #19619, #12909 ) ;
#9480 = DIRECTION ( 'NONE',  ( 0.08420877549337300871, 0.000000000000000000, 0.9964481331860212121 ) ) ;
#9481 = CARTESIAN_POINT ( 'NONE',  ( 39.00487391864218267, 37.69864044684034354, -3.894748490052650780 ) ) ;
#9482 = DIRECTION ( 'NONE',  ( -0.5285133232210438292, 0.8477492467026710443, 0.04466410071749180727 ) ) ;
#9483 = DIRECTION ( 'NONE',  ( 0.000000000000000000, -1.000000000000000000, -0.000000000000000000 ) ) ;
#9484 = CARTESIAN_POINT ( 'NONE',  ( 3.318611589506196058, 12.22314404142716171, 7.169435018240098323 ) ) ;
#9485 = ORIENTED_EDGE ( 'NONE', *, *, #8686, .F. ) ;
#9486 = LINE ( 'NONE', #21096, #9642 ) ;
#9487 = CARTESIAN_POINT ( 'NONE',  ( 8.231104565076774904, 2.698862664129421329, -16.60274868773344537 ) ) ;
#9488 = CARTESIAN_POINT ( 'NONE',  ( 53.00421038040393995, -4.569743463999999200, 6.511420152579801446 ) ) ;
#9489 = DIRECTION ( 'NONE',  ( 0.000000000000000000, 1.000000000000000000, 0.000000000000000000 ) ) ;
#9490 = ADVANCED_FACE ( 'NONE', ( #614 ), #14677, .F. ) ;
#9491 = VECTOR ( 'NONE', #20630, 1000.000000000000000 ) ;
#9492 = ORIENTED_EDGE ( 'NONE', *, *, #2600, .F. ) ;
#9493 = ORIENTED_EDGE ( 'NONE', *, *, #21422, .T. ) ;
#9494 = CARTESIAN_POINT ( 'NONE',  ( 10.96785682973680132, 15.74068497743424189, 7.058765615034965357 ) ) ;
#9496 = CARTESIAN_POINT ( 'NONE',  ( 50.62387473582167274, 34.52875999999999834, -28.41576006634952734 ) ) ;
#9495 = CARTESIAN_POINT ( 'NONE',  ( 12.88040283537677588, 38.48766750000000059, -0.09070320285213756550 ) ) ;
#9497 = CARTESIAN_POINT ( 'NONE',  ( 10.97135499597955821, 13.84880078443595153, -3.805639818675497388 ) ) ;
#9498 = VERTEX_POINT ( 'NONE', #6571 ) ;
#9499 = VERTEX_POINT ( 'NONE', #12904 ) ;
#9500 = CARTESIAN_POINT ( 'NONE',  ( 49.41195815393805901, 42.06303499999999929, -1.411525001868561224 ) ) ;
#9501 = EDGE_CURVE ( 'NONE', #7839, #20066, #7900, .T. ) ;
#9502 = VECTOR ( 'NONE', #12148, 1000.000000000000000 ) ;
#9503 = CARTESIAN_POINT ( 'NONE',  ( 8.013468311210377948, 20.40777636399528916, -1.234548792046807231 ) ) ;
#9504 = ADVANCED_FACE ( 'NONE', ( #16751 ), #18388, .F. ) ;
#9505 = CARTESIAN_POINT ( 'NONE',  ( 8.115152695261373950, 20.48792095732073548, 4.726086490775795568 ) ) ;
#9506 = AXIS2_PLACEMENT_3D ( 'NONE', #7258, #19180, #20609 ) ;
#9507 = CARTESIAN_POINT ( 'NONE',  ( 2.827233722371560454, 19.13019741901238646, 7.400779595140909883 ) ) ;
#9508 = AXIS2_PLACEMENT_3D ( 'NONE', #16199, #4791, #11523 ) ;
#9509 = CARTESIAN_POINT ( 'NONE',  ( 52.69765441554997665, -7.547610000000001484, -16.33112036207927886 ) ) ;
#9510 = CARTESIAN_POINT ( 'NONE',  ( 8.011380105705496746, -1.594802499999999013, -19.05252355006962617 ) ) ;
#9511 = CARTESIAN_POINT ( 'NONE',  ( 3.885025484994841793, 19.12622466589174053, -0.7968053903680345496 ) ) ;
#9512 = CARTESIAN_POINT ( 'NONE',  ( 1.698356033660393782, 15.60214721349694145, 9.558218796784109017 ) ) ;
#9513 = ORIENTED_EDGE ( 'NONE', *, *, #20383, .F. ) ;
#9514 = CARTESIAN_POINT ( 'NONE',  ( 3.007751381752465925, 20.19548487530456171, 2.160188886951264209 ) ) ;
#9515 = DIRECTION ( 'NONE',  ( -0.2490110332224850509, 0.000000000000000000, 0.9685006480810792739 ) ) ;
#9516 = CARTESIAN_POINT ( 'NONE',  ( 41.71184157647478230, 38.88803500000000213, -2.134205101306931862 ) ) ;
#9517 = CARTESIAN_POINT ( 'NONE',  ( 14.65261474522852936, -8.323537342180904020, -15.15547592125267151 ) ) ;
#9518 = EDGE_CURVE ( 'NONE', #17468, #12588, #8335, .T. ) ;
#9519 = ORIENTED_EDGE ( 'NONE', *, *, #6603, .T. ) ;
#9520 = DIRECTION ( 'NONE',  ( 0.000000000000000000, 1.000000000000000000, 0.000000000000000000 ) ) ;
#9521 = PRODUCT_RELATED_PRODUCT_CATEGORY ( 'part', '', ( #6509 ) ) ;
#9522 = VECTOR ( 'NONE', #6929, 1000.000000000000000 ) ;
#9523 = CARTESIAN_POINT ( 'NONE',  ( 9.163629188038463269, 17.17735727408968316, -3.567318444911117936 ) ) ;
#9524 = EDGE_LOOP ( 'NONE', ( #3744, #1077 ) ) ;
#9525 = CIRCLE ( 'NONE', #17292, 3.175000000000000711 ) ;
#9526 = CARTESIAN_POINT ( 'NONE',  ( -6.268352501591477832, -0.7997824999999986195, -35.49402737582407497 ) ) ;
#9527 = CARTESIAN_POINT ( 'NONE',  ( 12.70203135958802143, 21.28102902729012058, 0.03842769806917034625 ) ) ;
#9528 = CARTESIAN_POINT ( 'NONE',  ( 5.839807527371365659, 19.32544709538717953, -1.321624354577452420 ) ) ;
#9529 = CARTESIAN_POINT ( 'NONE',  ( 29.98909767165928386, 9.120187499999998337, -5.214162619065493054 ) ) ;
#9530 = CARTESIAN_POINT ( 'NONE',  ( 6.219149445766309903, 11.66082179432958377, 2.494857446435102322 ) ) ;
#9531 = ORIENTED_EDGE ( 'NONE', *, *, #2720, .T. ) ;
#9532 = CARTESIAN_POINT ( 'NONE',  ( 6.585898268469219552, 1.984375000000000000, 4.694966092919240275 ) ) ;
#9533 = VECTOR ( 'NONE', #17376, 1000.000000000000000 ) ;
#9534 = CARTESIAN_POINT ( 'NONE',  ( 18.07371581377308800, -1.983739999999999393, -11.95909761906105473 ) ) ;
#9535 = CARTESIAN_POINT ( 'NONE',  ( 7.835562974045392259, 21.09291897731618093, 3.110782529598515200 ) ) ;
#9536 = AXIS2_PLACEMENT_3D ( 'NONE', #7102, #19028, #7325 ) ;
#9537 = CARTESIAN_POINT ( 'NONE',  ( 38.46688692048027747, -5.391489964475852048, -4.537348303483145884 ) ) ;
#9538 = CARTESIAN_POINT ( 'NONE',  ( 1.335867332802413321, 21.11849136136308047, 3.284394833007574732 ) ) ;
#9539 = PLANE ( 'NONE',  #12828 ) ;
#9540 = CARTESIAN_POINT ( 'NONE',  ( 6.751191191974612593, 11.44921631601969203, 2.721930595337344716 ) ) ;
#9541 = DIRECTION ( 'NONE',  ( 0.000000000000000000, -1.000000000000000000, 0.000000000000000000 ) ) ;
#9542 = DIRECTION ( 'NONE',  ( 0.2868778675745011220, 0.000000000000000000, 0.9579671649362033747 ) ) ;
#9543 = EDGE_CURVE ( 'NONE', #1202, #15261, #19458, .T. ) ;
#9544 = EDGE_CURVE ( 'NONE', #5911, #14322, #9997, .T. ) ;
#9545 = FACE_OUTER_BOUND ( 'NONE', #2694, .T. ) ;
#9546 = VECTOR ( 'NONE', #5078, 1000.000000000000000 ) ;
#9547 = VERTEX_POINT ( 'NONE', #1593 ) ;
#9548 = CARTESIAN_POINT ( 'NONE',  ( 29.15193331460030279, 39.28205249999999893, -13.61707959051006966 ) ) ;
#9549 = DIRECTION ( 'NONE',  ( -0.9685006480810794960, 0.000000000000000000, -0.2490110332224836354 ) ) ;
#9550 = ORIENTED_EDGE ( 'NONE', *, *, #4239, .F. ) ;
#9551 = CARTESIAN_POINT ( 'NONE',  ( 10.16671340789460487, 20.24294540929401975, -1.062930679991952232 ) ) ;
#9552 = CARTESIAN_POINT ( 'NONE',  ( 28.56548256563643662, 36.51313500000000545, -12.12873025803960658 ) ) ;
#9553 = CARTESIAN_POINT ( 'NONE',  ( -0.1849527131266449076, 20.23672349358593792, 5.150944217628095068 ) ) ;
#9554 = CARTESIAN_POINT ( 'NONE',  ( 14.49583489321334007, -8.530823778528098700, -14.71411849925045523 ) ) ;
#9555 = AXIS2_PLACEMENT_3D ( 'NONE', #21160, #21381, #7579 ) ;
#9557 = CARTESIAN_POINT ( 'NONE',  ( 47.80475250345343596, 38.88803500000000213, -11.91473563638196786 ) ) ;
#9556 = CARTESIAN_POINT ( 'NONE',  ( -0.3117854395798596578, 15.69350566183319273, 0.7735685379110269766 ) ) ;
#9558 = ORIENTED_EDGE ( 'NONE', *, *, #16958, .T. ) ;
#9559 = LINE ( 'NONE', #6137, #5325 ) ;
#9560 = ORIENTED_EDGE ( 'NONE', *, *, #6778, .T. ) ;
#9561 = CARTESIAN_POINT ( 'NONE',  ( 19.62005440932008682, -0.3128815169959983655, -14.95834899907133142 ) ) ;
#9562 = VECTOR ( 'NONE', #10000, 1000.000000000000114 ) ;
#9563 = CIRCLE ( 'NONE', #18049, 30.16249999999999787 ) ;
#9564 = VERTEX_POINT ( 'NONE', #3146 ) ;
#9565 = CARTESIAN_POINT ( 'NONE',  ( 10.74157715189224049, 19.11273924176536099, 6.105315142739899947 ) ) ;
#9566 = CARTESIAN_POINT ( 'NONE',  ( 7.534728409618654865, 21.81389254086020202, 3.255105835292287697 ) ) ;
#9567 = EDGE_CURVE ( 'NONE', #2328, #18667, #20035, .T. ) ;
#9568 = CARTESIAN_POINT ( 'NONE',  ( 66.03921914090641110, -42.42568807200000691, -11.33033647675950029 ) ) ;
#9569 = ORIENTED_EDGE ( 'NONE', *, *, #14972, .T. ) ;
#9570 = LINE ( 'NONE', #16341, #2244 ) ;
#9571 = DIRECTION ( 'NONE',  ( 0.000000000000000000, 1.000000000000000000, 0.000000000000000000 ) ) ;
#9572 = CLOSED_SHELL ( 'NONE', ( #8205, #9269, #5297, #10454, #21226, #11126, #21776, #9490, #12256, #2133, #2499, #6952, #6646, #8791, #3073, #18308, #2671, #16928, #718, #20848, #15915, #12254, #8388, #3242, #5966, #21406, #19078, #17019, #10900, #18023, #18304, #17352, #11549, #14098, #5201, #12381, #11955, #3685, #13179, #14072, #575, #12106, #6433, #182, #15843, #10632, #1245, #4926, #6229, #10051, #20093, #16932, #1383, #1613, #19384, #13879, #1536, #12889, #3374, #4563, #19646, #10032, #14820, #19769, #14839, #2418, #7981, #10576, #14113, #719, #850, #1166, #14347, #8577, #19797, #18330, #15023, #13039, #18536, #11960, #9385, #14798, #6295, #7658, #12654, #12902, #12467, #5880, #17238, #14049, #3817, #7136, #9887, #2043, #8500, #4423, #1193, #10873, #9673, #5426, #16355, #20113, #10879, #9645, #7509, #10383, #4139, #13093, #16560, #715, #13295, #7773, #7331, #11387, #18399, #18278, #8706, #19402, #8022, #21148, #15237, #17452, #3347, #12083, #8624, #20047, #11459, #2195, #6384, #1277, #6975, #17645, #4592, #13149, #2049, #20079, #11432, #9070, #15049, #21054, #13902, #9652, #20437, #9594, #4648, #13611, #16815, #4003 ) ) ;
#9573 = ORIENTED_EDGE ( 'NONE', *, *, #20748, .T. ) ;
#9574 = EDGE_LOOP ( 'NONE', ( #21086, #6383, #7724, #15405 ) ) ;
#9575 = AXIS2_PLACEMENT_3D ( 'NONE', #19007, #455, #661 ) ;
#9576 = CARTESIAN_POINT ( 'NONE',  ( 34.72145145287101542, 2.586003464000000029, 0.5851394578805096947 ) ) ;
#9578 = LINE ( 'NONE', #13257, #7802 ) ;
#9577 = CARTESIAN_POINT ( 'NONE',  ( 1.577524075207264342, 16.44750854861721834, -0.7742535818055841235 ) ) ;
#9579 = ORIENTED_EDGE ( 'NONE', *, *, #4364, .T. ) ;
#9580 = CARTESIAN_POINT ( 'NONE',  ( 4.336475100890431200, 20.29160327599122837, 0.2727996324811496898 ) ) ;
#9581 = VERTEX_POINT ( 'NONE', #18285 ) ;
#9582 = CIRCLE ( 'NONE', #19460, 9.525000000000002132 ) ;
#9583 = ORIENTED_EDGE ( 'NONE', *, *, #3508, .F. ) ;
#9584 =( BOUNDED_CURVE ( )  B_SPLINE_CURVE ( 3, ( #3058, #1281, #12502, #11346 ),
 .UNSPECIFIED., .F., .T. ) 
 B_SPLINE_CURVE_WITH_KNOTS ( ( 4, 4 ),
 ( 0.000000000000000000, 1.570796326788112873 ),
 .UNSPECIFIED. ) 
 CURVE ( )  GEOMETRIC_REPRESENTATION_ITEM ( )  RATIONAL_B_SPLINE_CURVE ( ( 1.000000000000000000, 0.8047378541259639917, 0.8047378541259639917, 1.000000000000000000 ) ) 
 REPRESENTATION_ITEM ( '' )  );
#9585 = EDGE_LOOP ( 'NONE', ( #10385, #17245, #16552, #10834 ) ) ;
#9586 = VECTOR ( 'NONE', #14815, 1000.000000000000000 ) ;
#9587 = AXIS2_PLACEMENT_3D ( 'NONE', #11617, #14963, #18156 ) ;
#9588 = CIRCLE ( 'NONE', #21589, 0.5079999999999997851 ) ;
#9589 = LINE ( 'NONE', #14603, #5358 ) ;
#9590 = CARTESIAN_POINT ( 'NONE',  ( 39.93069333241970043, 38.72516837585681770, -3.008993689095889490 ) ) ;
#9591 = DIRECTION ( 'NONE',  ( -0.9685006480810792739, 0.000000000000000000, -0.2490110332224850231 ) ) ;
#9592 = CARTESIAN_POINT ( 'NONE',  ( 15.87579517430159193, 39.28205249999999893, -46.44757911220182223 ) ) ;
#9593 = CARTESIAN_POINT ( 'NONE',  ( 3.645750917779165157, 14.75475157674404691, 8.959486830434602922 ) ) ;
#9594 = ADVANCED_FACE ( 'NONE', ( #21278 ), #1265, .T. ) ;
#9595 = AXIS2_PLACEMENT_3D ( 'NONE', #11593, #10250, #4948 ) ;
#9596 = VECTOR ( 'NONE', #9757, 1000.000000000000000 ) ;
#9597 = ORIENTED_EDGE ( 'NONE', *, *, #1777, .F. ) ;
#9598 = DIRECTION ( 'NONE',  ( -0.5171931484643331745, 0.000000000000000000, -0.8558687090795820129 ) ) ;
#9599 = CARTESIAN_POINT ( 'NONE',  ( -15.39353573898878658, -2.254660308866960339, -10.30107656633069979 ) ) ;
#9600 = CARTESIAN_POINT ( 'NONE',  ( 13.64200589084435578, 38.48766750000000059, -0.3187768451312169571 ) ) ;
#9601 = CARTESIAN_POINT ( 'NONE',  ( -49.72082486877479113, 38.25938500000000175, -7.603226040068017610 ) ) ;
#9602 = FACE_OUTER_BOUND ( 'NONE', #21424, .T. ) ;
#9603 = ORIENTED_EDGE ( 'NONE', *, *, #10631, .F. ) ;
#9604 = ORIENTED_EDGE ( 'NONE', *, *, #8649, .F. ) ;
#9605 = CARTESIAN_POINT ( 'NONE',  ( 8.970099111347026977, 16.58550361725992772, 7.489321828938900083 ) ) ;
#9607 = DIRECTION ( 'NONE',  ( 0.000000000000000000, 1.000000000000000000, 0.000000000000000000 ) ) ;
#9606 = CARTESIAN_POINT ( 'NONE',  ( -29.36874999999999858, 32.54502000000000095, -3.968750000000000000 ) ) ;
#9608 = CARTESIAN_POINT ( 'NONE',  ( 11.11774465870644946, 12.58812117891224602, -3.039815099727486647 ) ) ;
#9609 = ORIENTED_EDGE ( 'NONE', *, *, #9501, .F. ) ;
#9610 = VECTOR ( 'NONE', #7992, 1000.000000000000000 ) ;
#9611 = ORIENTED_EDGE ( 'NONE', *, *, #454, .T. ) ;
#9612 = DIRECTION ( 'NONE',  ( 0.5222415575336524229, 0.000000000000000000, 0.8527976052879281399 ) ) ;
#9613 = CARTESIAN_POINT ( 'NONE',  ( 7.143155634628241657, 20.85017009081515127, 2.146504125371351268 ) ) ;
#9614 = VECTOR ( 'NONE', #392, 1000.000000000000114 ) ;
#9615 = CIRCLE ( 'NONE', #17768, 1.785937499999998179 ) ;
#9616 = EDGE_CURVE ( 'NONE', #20092, #9393, #6134, .T. ) ;
#9617 = CIRCLE ( 'NONE', #5052, 0.7950199999999985057 ) ;
#9618 = CARTESIAN_POINT ( 'NONE',  ( 13.68236715249897273, 22.02408774531873803, 1.842928636733466297 ) ) ;
#9619 = CARTESIAN_POINT ( 'NONE',  ( 21.03437500000000071, 1.984375000000000000, 5.159374999999999822 ) ) ;
#9620 = LINE ( 'NONE', #6089, #1407 ) ;
#9621 = CARTESIAN_POINT ( 'NONE',  ( 5.597898337543679048, 15.64116283607404689, 8.868322025159471877 ) ) ;
#9622 = CARTESIAN_POINT ( 'NONE',  ( 1.185536613426001029, 11.80994437923685325, 6.710694494223975681 ) ) ;
#9623 = EDGE_CURVE ( 'NONE', #15261, #7667, #8863, .T. ) ;
#9624 = CARTESIAN_POINT ( 'NONE',  ( 57.69402548289047417, 0.000000000000000000, -20.84562559047711261 ) ) ;
#9625 = EDGE_CURVE ( 'NONE', #5674, #7354, #14544, .T. ) ;
#9626 = EDGE_LOOP ( 'NONE', ( #3576, #2415, #1182, #14467 ) ) ;
#9627 = CARTESIAN_POINT ( 'NONE',  ( 3.488048491702187892, 16.48205525895868462, 8.498464847168406777 ) ) ;
#9628 = DIRECTION ( 'NONE',  ( 0.000000000000000000, -1.000000000000000000, -0.000000000000000000 ) ) ;
#9629 = DIRECTION ( 'NONE',  ( 0.9876802608827758290, 0.000000000000000000, -0.1564854698127972066 ) ) ;
#9630 = CARTESIAN_POINT ( 'NONE',  ( 14.60635709262053439, -8.313957965053235810, -15.16560502254627174 ) ) ;
#9631 = ORIENTED_EDGE ( 'NONE', *, *, #8761, .T. ) ;
#9632 = DIRECTION ( 'NONE',  ( 0.000000000000000000, 1.000000000000000000, 0.000000000000000000 ) ) ;
#9633 = CARTESIAN_POINT ( 'NONE',  ( 6.820530933416198316, 11.28301579719734171, 5.079670947778354595 ) ) ;
#9634 = AXIS2_PLACEMENT_3D ( 'NONE', #1895, #8525, #17048 ) ;
#9635 = CARTESIAN_POINT ( 'NONE',  ( 10.15167233650402423, 21.12619246702464437, -1.194501015968789881 ) ) ;
#9636 = ORIENTED_EDGE ( 'NONE', *, *, #15908, .T. ) ;
#9637 = DIRECTION ( 'NONE',  ( 0.000000000000000000, 1.000000000000000000, -0.000000000000000000 ) ) ;
#9638 = CARTESIAN_POINT ( 'NONE',  ( 7.512256438360484623, 21.70324290413769219, 3.137831150439451378 ) ) ;
#9639 = CARTESIAN_POINT ( 'NONE',  ( 9.275488759993784527, 40.07707250000000698, -20.77642327197297689 ) ) ;
#9640 = CARTESIAN_POINT ( 'NONE',  ( -0.6269647750601365921, 20.05113242023052322, 3.964184760248283368 ) ) ;
#9641 = FILL_AREA_STYLE_COLOUR ( '', #13464 ) ;
#9642 = VECTOR ( 'NONE', #19654, 1000.000000000000114 ) ;
#9643 = CARTESIAN_POINT ( 'NONE',  ( 6.490352011916383113, 19.85778700119437445, 5.984496968252292604 ) ) ;
#9644 = DIRECTION ( 'NONE',  ( -0.9685006480810792739, 0.000000000000000000, -0.2490110332224846346 ) ) ;
#9645 = ADVANCED_FACE ( 'NONE', ( #9769 ), #4588, .T. ) ;
#9646 = CIRCLE ( 'NONE', #116, 30.16249999999999076 ) ;
#9647 = CARTESIAN_POINT ( 'NONE',  ( 8.122941931605208055, 11.97223945099518083, 0.1250674085377973255 ) ) ;
#9648 = CARTESIAN_POINT ( 'NONE',  ( 5.182497302550231666, 17.60298196088504952, 7.859483784311269261 ) ) ;
#9649 = CARTESIAN_POINT ( 'NONE',  ( 23.41562500000000213, 30.56064500000000095, 5.159374999999999822 ) ) ;
#9650 = CARTESIAN_POINT ( 'NONE',  ( 2.972756920594751495, 11.23314441701904087, 5.199616837626352073 ) ) ;
#9651 = CARTESIAN_POINT ( 'NONE',  ( -1.351150467732365579, 2.373947500000000765, -27.17319717629097653 ) ) ;
#9652 = ADVANCED_FACE ( 'NONE', ( #18080 ), #2940, .T. ) ;
#9653 = CARTESIAN_POINT ( 'NONE',  ( 32.18388890846549799, 29.95901653600000003, 1.507793899792891468 ) ) ;
#9654 = CARTESIAN_POINT ( 'NONE',  ( 6.664121936844724203, 11.05293067483325054, 2.719061972016084461 ) ) ;
#9655 = DIRECTION ( 'NONE',  ( 0.000000000000000000, 1.000000000000000000, 0.000000000000000000 ) ) ;
#9656 = CARTESIAN_POINT ( 'NONE',  ( 20.14654830070027813, -6.335923874353329488, -15.19130692721172515 ) ) ;
#9657 = CIRCLE ( 'NONE', #16727, 11.02160133116777985 ) ;
#9658 = CARTESIAN_POINT ( 'NONE',  ( 65.04486224192415023, -1.983739999999999393, -32.83524980818705785 ) ) ;
#9659 = ORIENTED_EDGE ( 'NONE', *, *, #943, .F. ) ;
#9660 = CARTESIAN_POINT ( 'NONE',  ( 23.49608546833631451, 3.565842500000000914, -17.12016812500874252 ) ) ;
#9661 = CARTESIAN_POINT ( 'NONE',  ( -15.41509608936259035, 37.15413452960619622, -10.31276839742836415 ) ) ;
#9662 = EDGE_LOOP ( 'NONE', ( #7208, #17310, #10739, #27 ) ) ;
#9663 = CARTESIAN_POINT ( 'NONE',  ( 12.47845653567284252, 19.78773270843656107, 5.077144801013766084 ) ) ;
#9664 = CARTESIAN_POINT ( 'NONE',  ( 11.72582454026615828, -4.501321389889026747, -15.56411338575258974 ) ) ;
#9665 = DIRECTION ( 'NONE',  ( 0.000000000000000000, -1.000000000000000000, 0.000000000000000000 ) ) ;
#9666 = ORIENTED_EDGE ( 'NONE', *, *, #18993, .T. ) ;
#9667 = CARTESIAN_POINT ( 'NONE',  ( 38.95211873669086344, -5.166601264346659228, -3.952980512833436322 ) ) ;
#9668 = CARTESIAN_POINT ( 'NONE',  ( -3.037751992662818257, 28.56769750000000130, -30.02724401157551526 ) ) ;
#9669 = ORIENTED_EDGE ( 'NONE', *, *, #14654, .T. ) ;
#9670 = CARTESIAN_POINT ( 'NONE',  ( 19.39617148027078741, 0.1681879138596751311, -15.03931347124663453 ) ) ;
#9671 = EDGE_CURVE ( 'NONE', #13654, #14268, #16535, .T. ) ;
#9672 = VECTOR ( 'NONE', #4542, 1000.000000000000000 ) ;
#9673 = ADVANCED_FACE ( 'NONE', ( #21605 ), #6467, .T. ) ;
#9674 = EDGE_CURVE ( 'NONE', #1021, #7959, #10989, .T. ) ;
#9675 = CARTESIAN_POINT ( 'NONE',  ( 19.75185127208544600, 0.1555953079926848670, -15.00720622995094189 ) ) ;
#9676 = ORIENTED_EDGE ( 'NONE', *, *, #3726, .F. ) ;
#9677 = CARTESIAN_POINT ( 'NONE',  ( 11.28320163957777034, 21.35754284105190237, 1.995920704044074734 ) ) ;
#9678 = CARTESIAN_POINT ( 'NONE',  ( -23.01875000000000071, 0.000000000000000000, -10.31874999999999964 ) ) ;
#9679 = CARTESIAN_POINT ( 'NONE',  ( 9.071664746958145287, 21.95697059135326512, 1.680270923673110817 ) ) ;
#9680 = AXIS2_PLACEMENT_3D ( 'NONE', #14760, #19917, #8088 ) ;
#9681 = CARTESIAN_POINT ( 'NONE',  ( 19.13386765903375775, -5.735230366684957559, -15.44418781123290429 ) ) ;
#9682 = SURFACE_STYLE_USAGE ( .BOTH. , #11785 ) ;
#9683 = VERTEX_POINT ( 'NONE', #10319 ) ;
#9684 = DIRECTION ( 'NONE',  ( 0.000000000000000000, -1.000000000000000000, 0.000000000000000000 ) ) ;
#9685 = LINE ( 'NONE', #12922, #6392 ) ;
#9686 = AXIS2_PLACEMENT_3D ( 'NONE', #20481, #18838, #10447 ) ;
#9687 = VERTEX_POINT ( 'NONE', #8655 ) ;
#9688 = VERTEX_POINT ( 'NONE', #11773 ) ;
#9689 = CARTESIAN_POINT ( 'NONE',  ( 17.93242123830337320, -8.292540772221606460, -14.39788784616911776 ) ) ;
#9691 = CARTESIAN_POINT ( 'NONE',  ( -160.2647810241784896, 30.56128000000000000, 8.731885000000000119 ) ) ;
#9690 = CARTESIAN_POINT ( 'NONE',  ( 7.484288373972455943, 14.71660677864375799, 8.297660023429632048 ) ) ;
#9692 = ORIENTED_EDGE ( 'NONE', *, *, #17786, .F. ) ;
#9693 = CARTESIAN_POINT ( 'NONE',  ( 4.110461435211806958, 11.46719836097712175, 1.771832583802136485 ) ) ;
#9694 = ORIENTED_EDGE ( 'NONE', *, *, #26, .F. ) ;
#9695 = ORIENTED_EDGE ( 'NONE', *, *, #11173, .T. ) ;
#9696 = VECTOR ( 'NONE', #13921, 1000.000000000000000 ) ;
#9697 = CARTESIAN_POINT ( 'NONE',  ( 0.7209684937559326379, 12.21855677317197042, 4.661992077991788719 ) ) ;
#9698 = EDGE_CURVE ( 'NONE', #19545, #16113, #16600, .T. ) ;
#9699 = ORIENTED_EDGE ( 'NONE', *, *, #13846, .F. ) ;
#9700 = CIRCLE ( 'NONE', #10787, 3.175000000000000711 ) ;
#9701 = FACE_OUTER_BOUND ( 'NONE', #113, .T. ) ;
#9702 = DIRECTION ( 'NONE',  ( 0.000000000000000000, 1.000000000000000000, 0.000000000000000000 ) ) ;
#9703 = DIRECTION ( 'NONE',  ( -0.4987171968201974948, 0.000000000000000000, 0.8667647648559581031 ) ) ;
#9704 = CARTESIAN_POINT ( 'NONE',  ( -46.55773479047372376, 38.26001999999999725, -7.870535429687039120 ) ) ;
#9705 = CARTESIAN_POINT ( 'NONE',  ( 3.652517087777511495, 15.28827823227851823, 9.103988936570855728 ) ) ;
#9706 = ORIENTED_EDGE ( 'NONE', *, *, #9116, .F. ) ;
#9707 = FACE_OUTER_BOUND ( 'NONE', #16370, .T. ) ;
#9708 = CARTESIAN_POINT ( 'NONE',  ( 19.99312429566830218, 34.52875999999999834, -11.46559883803463720 ) ) ;
#9709 = LINE ( 'NONE', #1307, #9242 ) ;
#9710 = SURFACE_STYLE_FILL_AREA ( #7623 ) ;
#9711 = CARTESIAN_POINT ( 'NONE',  ( 18.65312499999999929, 32.54502000000000095, 5.159374999999999822 ) ) ;
#9712 = B_SPLINE_CURVE_WITH_KNOTS ( 'NONE', 3,
 ( #6932, #20510, #2055, #17444, #2173, #13695, #3843, #18640 ),
 .UNSPECIFIED., .F., .F.,
 ( 4, 2, 2, 4 ),
 ( 0.000000000000000000, 0.2500000000000000000, 0.5000000000000000000, 1.000000000000000000 ),
 .UNSPECIFIED. ) ;
#9713 = EDGE_LOOP ( 'NONE', ( #5856, #16788, #2296, #12913 ) ) ;
#9714 = VERTEX_POINT ( 'NONE', #366 ) ;
#9715 = CARTESIAN_POINT ( 'NONE',  ( 12.43409603417085840, 21.88443657126030217, 0.5679272856640997791 ) ) ;
#9716 = DIRECTION ( 'NONE',  ( 0.7421532822901579785, 0.000000000000000000, -0.6702301885068630005 ) ) ;
#9717 = CARTESIAN_POINT ( 'NONE',  ( 10.94319742441099130, 16.17454428140013789, -4.347327864958337784 ) ) ;
#9718 = ORIENTED_EDGE ( 'NONE', *, *, #1432, .F. ) ;
#9719 = VECTOR ( 'NONE', #14546, 1000.000000000000114 ) ;
#9720 = VERTEX_POINT ( 'NONE', #5224 ) ;
#9721 = LINE ( 'NONE', #4862, #18028 ) ;
#9722 = FACE_OUTER_BOUND ( 'NONE', #9713, .T. ) ;
#9723 = CARTESIAN_POINT ( 'NONE',  ( 9.221739120490575203, 16.47952005171203638, 7.223770130881796092 ) ) ;
#9724 = EDGE_CURVE ( 'NONE', #13886, #15003, #13653, .T. ) ;
#9725 = DIRECTION ( 'NONE',  ( -0.08420877549337300871, 0.000000000000000000, -0.9964481331860212121 ) ) ;
#9726 = CARTESIAN_POINT ( 'NONE',  ( 13.66532433034244320, 22.04443180264593138, 1.851018102324262227 ) ) ;
#9727 = DIRECTION ( 'NONE',  ( 0.000000000000000000, 1.000000000000000000, 0.000000000000000000 ) ) ;
#9728 = DIRECTION ( 'NONE',  ( 0.000000000000000000, 1.000000000000000000, 0.000000000000000000 ) ) ;
#9729 = CARTESIAN_POINT ( 'NONE',  ( 5.331667582216989665, 12.35064203674882144, 7.190230353468857416 ) ) ;
#9730 = CARTESIAN_POINT ( 'NONE',  ( 0.3826712150604609786, 11.72341736596831119, 3.192093716112220037 ) ) ;
#9731 = DIRECTION ( 'NONE',  ( 0.000000000000000000, -1.000000000000000000, 0.000000000000000000 ) ) ;
#9732 = ORIENTED_EDGE ( 'NONE', *, *, #15694, .F. ) ;
#9733 = CARTESIAN_POINT ( 'NONE',  ( 2.289123268938977773, 12.53619568343860102, 2.127697637126212626 ) ) ;
#9734 = LINE ( 'NONE', #20105, #4999 ) ;
#9735 = CARTESIAN_POINT ( 'NONE',  ( 20.88318715027774530, -3.948290930238875784, -13.86799592610689658 ) ) ;
#9736 = DIRECTION ( 'NONE',  ( -0.9767031480033346869, 0.000000000000000000, 0.2145948757085690273 ) ) ;
#9737 = ORIENTED_EDGE ( 'NONE', *, *, #6648, .F. ) ;
#9738 = FACE_OUTER_BOUND ( 'NONE', #6963, .T. ) ;
#9739 = CARTESIAN_POINT ( 'NONE',  ( 11.38283456236634983, 15.66465130118744398, 7.689368460568949182 ) ) ;
#9740 = CARTESIAN_POINT ( 'NONE',  ( 9.449104951163006305, 19.05165199613717419, -2.994418371723121197 ) ) ;
#9741 = ORIENTED_EDGE ( 'NONE', *, *, #21259, .F. ) ;
#9742 = CARTESIAN_POINT ( 'NONE',  ( 8.199318354130985753, 21.22306264867357939, 5.015000832792440022 ) ) ;
#9743 = CARTESIAN_POINT ( 'NONE',  ( 30.24348838687780727, 32.54502000000000095, -20.27293523655082552 ) ) ;
#9744 = CARTESIAN_POINT ( 'NONE',  ( 3.377149599728166862, 13.61484622919644139, 7.603189621071223314 ) ) ;
#9745 = DIRECTION ( 'NONE',  ( 0.000000000000000000, 0.000000000000000000, 1.000000000000000000 ) ) ;
#9746 = ADVANCED_FACE ( 'NONE', ( #6670 ), #17064, .T. ) ;
#9747 = ADVANCED_FACE ( 'NONE', ( #16849 ), #255, .T. ) ;
#9748 = DIRECTION ( 'NONE',  ( -0.6287118719681937806, 0.000000000000000000, -0.7776383362760928009 ) ) ;
#9749 = FACE_OUTER_BOUND ( 'NONE', #305, .T. ) ;
#9750 = CARTESIAN_POINT ( 'NONE',  ( 8.814777221004259644, 20.70901284984930157, 0.06808976589407680913 ) ) ;
#9751 = CARTESIAN_POINT ( 'NONE',  ( 5.276951256079190244, 16.94228911491327594, 8.002382959928944217 ) ) ;
#9752 = CARTESIAN_POINT ( 'NONE',  ( 5.897833037357203878, 15.65151869617330682, 8.688657562670337953 ) ) ;
#9753 = CARTESIAN_POINT ( 'NONE',  ( 28.38195592936287781, 39.28205249999999893, -13.81504834214261024 ) ) ;
#9754 = DIRECTION ( 'NONE',  ( 0.000000000000000000, -1.000000000000000000, 0.000000000000000000 ) ) ;
#9755 = CARTESIAN_POINT ( 'NONE',  ( 6.657844012983366255, 11.04603686758454018, 2.720439051447127721 ) ) ;
#9756 = CARTESIAN_POINT ( 'NONE',  ( 24.43309469626978725, 23.18727947754285879, -0.6496488801123181389 ) ) ;
#9757 = DIRECTION ( 'NONE',  ( 0.000000000000000000, 1.000000000000000000, 0.000000000000000000 ) ) ;
#9758 = DIRECTION ( 'NONE',  ( 0.9685006480810794960, 0.000000000000000000, 0.2490110332224836354 ) ) ;
#9759 = ORIENTED_EDGE ( 'NONE', *, *, #14971, .T. ) ;
#9760 = DIRECTION ( 'NONE',  ( -0.2227372614607789347, 0.000000000000000000, -0.9748785115884710528 ) ) ;
#9761 = EDGE_CURVE ( 'NONE', #97, #19859, #746, .T. ) ;
#9762 = CYLINDRICAL_SURFACE ( 'NONE', #21413, 0.7950200000000000600 ) ;
#9763 = ORIENTED_EDGE ( 'NONE', *, *, #15205, .T. ) ;
#9764 = CARTESIAN_POINT ( 'NONE',  ( 9.434918120449587775, 17.44535875574114314, -2.750588363923260893 ) ) ;
#9765 = DIRECTION ( 'NONE',  ( -1.000000000000000000, 0.000000000000000000, 0.000000000000000000 ) ) ;
#9766 = VECTOR ( 'NONE', #14995, 1000.000000000000114 ) ;
#9767 = DIRECTION ( 'NONE',  ( 0.000000000000000000, 1.000000000000000000, 0.000000000000000000 ) ) ;
#9768 = CARTESIAN_POINT ( 'NONE',  ( 20.01377712881487980, -2.741521743599813821, -13.99508467333011907 ) ) ;
#9769 = FACE_OUTER_BOUND ( 'NONE', #4959, .T. ) ;
#9770 = EDGE_LOOP ( 'NONE', ( #19568, #2966, #3285, #3823 ) ) ;
#9771 = CARTESIAN_POINT ( 'NONE',  ( 38.94885947252404179, -5.166721542084396823, -3.956611957468594287 ) ) ;
#9772 = CARTESIAN_POINT ( 'NONE',  ( 66.87634738983680904, 1.984375000000000000, 3.497859541731999755 ) ) ;
#9773 = EDGE_CURVE ( 'NONE', #624, #13225, #1910, .T. ) ;
#9774 = ORIENTED_EDGE ( 'NONE', *, *, #9226, .F. ) ;
#9775 = EDGE_CURVE ( 'NONE', #16183, #11029, #1400, .T. ) ;
#9776 = CARTESIAN_POINT ( 'NONE',  ( 201.9384738932629944, 1.984375000000000000, 10.71562489836746046 ) ) ;
#9777 = ORIENTED_EDGE ( 'NONE', *, *, #2953, .F. ) ;
#9778 = CARTESIAN_POINT ( 'NONE',  ( 7.810570628557063522, 12.04767321495844179, 0.2632024995130942124 ) ) ;
#9779 = CARTESIAN_POINT ( 'NONE',  ( 2.929006426436138621, 20.11622341764773125, 2.226180933043676369 ) ) ;
#9780 = CARTESIAN_POINT ( 'NONE',  ( 38.86292893166786655, 40.07865999999999929, -4.051696374780784815 ) ) ;
#9781 = CARTESIAN_POINT ( 'NONE',  ( 7.419152651973274004, 18.37230293632699230, -2.654332437207524542 ) ) ;
#9782 = AXIS2_PLACEMENT_3D ( 'NONE', #12582, #9130, #9241 ) ;
#9783 = VERTEX_POINT ( 'NONE', #13545 ) ;
#9784 = CARTESIAN_POINT ( 'NONE',  ( 9.160622857117788342, 21.06163945996668119, 1.886083935128181732 ) ) ;
#9785 = CARTESIAN_POINT ( 'NONE',  ( 9.810057962265917197, 21.83905339296156356, 3.589454503528180851 ) ) ;
#9786 = EDGE_CURVE ( 'NONE', #3005, #21819, #13780, .T. ) ;
#9787 = DIRECTION ( 'NONE',  ( 0.000000000000000000, 1.000000000000000000, 0.000000000000000000 ) ) ;
#9788 = ORIENTED_EDGE ( 'NONE', *, *, #7590, .T. ) ;
#9789 = EDGE_CURVE ( 'NONE', #16977, #535, #146, .T. ) ;
#9790 = VERTEX_POINT ( 'NONE', #18824 ) ;
#9791 = EDGE_CURVE ( 'NONE', #15606, #9720, #20101, .T. ) ;
#9792 = CYLINDRICAL_SURFACE ( 'NONE', #14133, 3.968750000000000000 ) ;
#9794 = DIRECTION ( 'NONE',  ( 0.000000000000000000, -1.000000000000000000, 0.000000000000000000 ) ) ;
#9793 = CARTESIAN_POINT ( 'NONE',  ( 5.392306785532915647, 17.51139020089073028, 8.808111370990710398 ) ) ;
#9795 = VERTEX_POINT ( 'NONE', #16949 ) ;
#9796 = CARTESIAN_POINT ( 'NONE',  ( 5.682439063020419567, 21.52104170944363304, 3.898124636232009887 ) ) ;
#9797 = EDGE_LOOP ( 'NONE', ( #18313, #19205, #11212, #6189 ) ) ;
#9798 = CIRCLE ( 'NONE', #16192, 3.970019999999997662 ) ;
#9799 = ORIENTED_EDGE ( 'NONE', *, *, #5708, .F. ) ;
#9800 = DIRECTION ( 'NONE',  ( 0.000000000000000000, 1.000000000000000000, 0.000000000000000000 ) ) ;
#9801 = ORIENTED_EDGE ( 'NONE', *, *, #896, .F. ) ;
#9802 = CARTESIAN_POINT ( 'NONE',  ( 7.305327845366293538, 16.38034437524489206, -3.033659931233324780 ) ) ;
#9803 = CARTESIAN_POINT ( 'NONE',  ( 4.541085437132517555, 11.87214774573713072, 3.616631113229732630 ) ) ;
#9804 = CARTESIAN_POINT ( 'NONE',  ( 12.57635667311951622, -95.96551800000000298, 1.354834321244424267 ) ) ;
#9805 = DIRECTION ( 'NONE',  ( -0.8667647648559581031, 0.000000000000000000, -0.4987171968201974948 ) ) ;
#9806 = DIRECTION ( 'NONE',  ( 0.9129422336036122632, 0.000000000000000000, -0.4080888115384288528 ) ) ;
#9807 = CARTESIAN_POINT ( 'NONE',  ( 1.681618954495248675, 14.37681556892286672, -0.2945994921972525660 ) ) ;
#9808 = AXIS2_PLACEMENT_3D ( 'NONE', #14189, #7637, #20897 ) ;
#9809 = VERTEX_POINT ( 'NONE', #7969 ) ;
#9810 = DIRECTION ( 'NONE',  ( 0.000000000000000000, -1.000000000000000000, -0.000000000000000000 ) ) ;
#9811 = DIRECTION ( 'NONE',  ( 0.7532174416907898573, 0.000000000000000000, 0.6577716059034334206 ) ) ;
#9812 = CARTESIAN_POINT ( 'NONE',  ( 54.36523883999320361, 32.54502000000000095, -30.28170612544299800 ) ) ;
#9813 = EDGE_CURVE ( 'NONE', #16186, #10813, #19351, .T. ) ;
#9814 = DIRECTION ( 'NONE',  ( -0.000000000000000000, -1.000000000000000000, 0.000000000000000000 ) ) ;
#9815 = ORIENTED_EDGE ( 'NONE', *, *, #4129, .F. ) ;
#9816 = EDGE_CURVE ( 'NONE', #877, #9895, #11613, .T. ) ;
#9817 = ORIENTED_EDGE ( 'NONE', *, *, #16520, .F. ) ;
#9818 = CARTESIAN_POINT ( 'NONE',  ( 12.19061143484422693, 20.00510796315846207, 5.223859247015660401 ) ) ;
#9819 = DIRECTION ( 'NONE',  ( 0.000000000000000000, 1.000000000000000000, 0.000000000000000000 ) ) ;
#9820 = ORIENTED_EDGE ( 'NONE', *, *, #11578, .T. ) ;
#9821 = ORIENTED_EDGE ( 'NONE', *, *, #9268, .T. ) ;
#9822 = CARTESIAN_POINT ( 'NONE',  ( 38.78586790977450960, 38.88803500000000213, -5.374168024304902147 ) ) ;
#9823 = CARTESIAN_POINT ( 'NONE',  ( 9.271480332380841460, 14.99039246332198161, 7.037024090030830514 ) ) ;
#9824 = AXIS2_PLACEMENT_3D ( 'NONE', #20221, #21882, #19903 ) ;
#9825 = CIRCLE ( 'NONE', #3859, 0.3962400000000008138 ) ;
#9826 = CARTESIAN_POINT ( 'NONE',  ( 1.532169971477637782, -1.500984687155947128, -20.71839214105750315 ) ) ;
#9827 = CARTESIAN_POINT ( 'NONE',  ( 2.447283566927735521, 20.82590581279646003, 6.632765824531373866 ) ) ;
#9828 = CARTESIAN_POINT ( 'NONE',  ( -0.08080654846667670310, 17.19714183529146112, 0.1023781220830352751 ) ) ;
#9829 = LINE ( 'NONE', #16599, #10150 ) ;
#9830 = VERTEX_POINT ( 'NONE', #4971 ) ;
#9831 = CARTESIAN_POINT ( 'NONE',  ( 0.1025994048457898045, 15.70581984897159700, 0.7443030867468957146 ) ) ;
#9832 = LINE ( 'NONE', #13726, #5709 ) ;
#9833 = DIRECTION ( 'NONE',  ( 1.000000000000000000, 0.000000000000000000, 0.000000000000000000 ) ) ;
#9834 = CARTESIAN_POINT ( 'NONE',  ( 18.23145731651337087, -7.767129607868482388, -14.37336575840138231 ) ) ;
#9835 = CARTESIAN_POINT ( 'NONE',  ( 42.35466991749225940, -9.531985000000000596, -17.94967221382040279 ) ) ;
#9836 = ORIENTED_EDGE ( 'NONE', *, *, #17897, .T. ) ;
#9837 = EDGE_CURVE ( 'NONE', #5914, #4928, #9829, .T. ) ;
#9838 = CARTESIAN_POINT ( 'NONE',  ( 13.33071950116100268, 14.65422691944639766, 7.092272786231333725 ) ) ;
#9839 = TOROIDAL_SURFACE ( 'NONE', #1716, 3.174999999999999822, 1.190625000000000044 ) ;
#9840 = CARTESIAN_POINT ( 'NONE',  ( 9.069792414751740139, 15.30434770100906583, -3.519768623950751962 ) ) ;
#9841 = ORIENTED_EDGE ( 'NONE', *, *, #8390, .F. ) ;
#9842 = CARTESIAN_POINT ( 'NONE',  ( 8.228154533012041583, 21.18466597396383122, 5.092860201889320315 ) ) ;
#9843 = CARTESIAN_POINT ( 'NONE',  ( 46.03750000000000142, -9.531985000000000596, -10.31874999999999964 ) ) ;
#9844 = CARTESIAN_POINT ( 'NONE',  ( 2.215916090217208811, 12.53249658949568257, 2.147356924360437347 ) ) ;
#9845 = DIRECTION ( 'NONE',  ( -0.2868778675745011220, 0.000000000000000000, -0.9579671649362034858 ) ) ;
#9846 = CARTESIAN_POINT ( 'NONE',  ( 6.975053525790806397, 18.43057135737701557, 7.137171834206872845 ) ) ;
#9847 = LINE ( 'NONE', #6761, #12894 ) ;
#9848 = VERTEX_POINT ( 'NONE', #2891 ) ;
#9849 = CARTESIAN_POINT ( 'NONE',  ( 7.333616852562694355, 21.20305659848830260, 1.380139826252072544 ) ) ;
#9850 = DIRECTION ( 'NONE',  ( 0.000000000000000000, 1.000000000000000000, 0.000000000000000000 ) ) ;
#9851 = CARTESIAN_POINT ( 'NONE',  ( 4.230681095848447981, 19.07995194538682071, -0.8237946677768968051 ) ) ;
#9852 = DIRECTION ( 'NONE',  ( 0.000000000000000000, 1.000000000000000000, 0.000000000000000000 ) ) ;
#9853 = DIRECTION ( 'NONE',  ( 0.9579671649362033747, 0.000000000000000000, -0.2868778675745006779 ) ) ;
#9854 = CIRCLE ( 'NONE', #13416, 3.968750000000000000 ) ;
#9855 = CARTESIAN_POINT ( 'NONE',  ( 6.622772524087491064, 11.63697146549233175, 2.774099957634049485 ) ) ;
#9856 = LINE ( 'NONE', #18489, #3382 ) ;
#9857 = DIRECTION ( 'NONE',  ( 0.000000000000000000, 1.000000000000000000, 0.000000000000000000 ) ) ;
#9858 = AXIS2_PLACEMENT_3D ( 'NONE', #2591, #6001, #1346 ) ;
#9859 = CARTESIAN_POINT ( 'NONE',  ( 26.59062499999999929, 26.59189500000000095, 8.731249999999999289 ) ) ;
#9860 = ADVANCED_FACE ( 'NONE', ( #19784 ), #16809, .T. ) ;
#9861 = ORIENTED_EDGE ( 'NONE', *, *, #20170, .T. ) ;
#9862 = DIRECTION ( 'NONE',  ( -0.9790635044817342925, 0.000000000000000000, 0.2035550397114870846 ) ) ;
#9863 = CYLINDRICAL_SURFACE ( 'NONE', #19999, 1.785937499999999512 ) ;
#9864 = ORIENTED_EDGE ( 'NONE', *, *, #570, .F. ) ;
#9865 = CARTESIAN_POINT ( 'NONE',  ( 12.97874336893425706, 17.75432315407044115, 6.220344854898855580 ) ) ;
#9866 = AXIS2_PLACEMENT_3D ( 'NONE', #3939, #5910, #5580 ) ;
#9867 = CARTESIAN_POINT ( 'NONE',  ( -47.86049599909252805, 38.25938500000000175, -23.29373766372935961 ) ) ;
#9868 = CARTESIAN_POINT ( 'NONE',  ( 19.42376837693508307, -5.426032880614602760, -13.68790637948557887 ) ) ;
#9870 = DIRECTION ( 'NONE',  ( 0.000000000000000000, 1.000000000000000000, 0.000000000000000000 ) ) ;
#9869 = CARTESIAN_POINT ( 'NONE',  ( 6.345766176488893073, 19.80783775455006435, 6.883578900750740637 ) ) ;
#9871 = ORIENTED_EDGE ( 'NONE', *, *, #17796, .T. ) ;
#9872 = PLANE ( 'NONE',  #6389 ) ;
#9873 = LINE ( 'NONE', #21388, #14804 ) ;
#9874 = ORIENTED_EDGE ( 'NONE', *, *, #7461, .T. ) ;
#9875 = VECTOR ( 'NONE', #2569, 1000.000000000000000 ) ;
#9876 = CARTESIAN_POINT ( 'NONE',  ( 31.75000000000000000, 1.984375000000000000, -4.317999999999999616 ) ) ;
#9877 =( GEOMETRIC_REPRESENTATION_CONTEXT ( 3 ) GLOBAL_UNCERTAINTY_ASSIGNED_CONTEXT ( ( #8771 ) ) GLOBAL_UNIT_ASSIGNED_CONTEXT ( ( #19730, #1382, #3280 ) ) REPRESENTATION_CONTEXT ( 'NONE', 'WORKASPACE' ) );
#9878 = CARTESIAN_POINT ( 'NONE',  ( 11.36393682984004450, -4.708245059028417501, -16.48153251965310062 ) ) ;
#9879 = EDGE_LOOP ( 'NONE', ( #13562, #8396, #9270, #15330 ) ) ;
#9880 = CARTESIAN_POINT ( 'NONE',  ( 7.421646152376969674, 16.36412484890491115, -2.219134118317299453 ) ) ;
#9881 = CARTESIAN_POINT ( 'NONE',  ( 2.323847236009109363, 18.74019614820905844, 0.7500644698246852204 ) ) ;
#9882 = ADVANCED_FACE ( 'NONE', ( #6303 ), #4658, .T. ) ;
#9883 = CARTESIAN_POINT ( 'NONE',  ( 16.85197508397059707, 13.08957250000000094, -16.77951971243562923 ) ) ;
#9884 = CARTESIAN_POINT ( 'NONE',  ( 14.32333359816743545, 21.25787525723532312, 4.225508590508356477 ) ) ;
#9885 = CARTESIAN_POINT ( 'NONE',  ( 18.94865055687374422, -5.956368045175373993, -15.47817826132612140 ) ) ;
#9886 = FACE_OUTER_BOUND ( 'NONE', #664, .T. ) ;
#9887 = ADVANCED_FACE ( 'NONE', ( #19678 ), #4546, .F. ) ;
#9888 = VERTEX_POINT ( 'NONE', #4869 ) ;
#9889 = EDGE_CURVE ( 'NONE', #12065, #14993, #21807, .T. ) ;
#9890 = EDGE_CURVE ( 'NONE', #9790, #17754, #14059, .T. ) ;
#9891 = CIRCLE ( 'NONE', #1029, 3.970019999999997662 ) ;
#9892 = CARTESIAN_POINT ( 'NONE',  ( 8.528587150289741459, 20.51903841992993804, 0.2064127866254405752 ) ) ;
#9893 = CARTESIAN_POINT ( 'NONE',  ( 9.547366781245800738, 14.64601895156848776, 7.841215834693419318 ) ) ;
#9894 = LINE ( 'NONE', #4927, #19105 ) ;
#9895 = VERTEX_POINT ( 'NONE', #9624 ) ;
#9896 = ORIENTED_EDGE ( 'NONE', *, *, #14904, .F. ) ;
#9897 = CARTESIAN_POINT ( 'NONE',  ( 61.65536943582333151, 0.000000000000000000, -11.98363747855214712 ) ) ;
#9899 = DIRECTION ( 'NONE',  ( 0.000000000000000000, 0.000000000000000000, 1.000000000000000000 ) ) ;
#9898 = CARTESIAN_POINT ( 'NONE',  ( 4.577338190742489488, 20.54266468784728161, 6.875769498540509339 ) ) ;
#9900 = ORIENTED_EDGE ( 'NONE', *, *, #3460, .T. ) ;
#9901 = CARTESIAN_POINT ( 'NONE',  ( 7.458443779878670021, 17.00624882743432664, 8.354293789368067991 ) ) ;
#9902 = VECTOR ( 'NONE', #4284, 1000.000000000000000 ) ;
#9903 = VERTEX_POINT ( 'NONE', #16389 ) ;
#9904 = VECTOR ( 'NONE', #839, 1000.000000000000227 ) ;
#9905 = VERTEX_POINT ( 'NONE', #8185 ) ;
#9906 = AXIS2_PLACEMENT_3D ( 'NONE', #6700, #13915, #20494 ) ;
#9907 = CARTESIAN_POINT ( 'NONE',  ( 0.1909874692627008541, 13.30835273160345800, 2.114876548789060173 ) ) ;
#9908 = PLANE ( 'NONE',  #19888 ) ;
#9909 = ORIENTED_EDGE ( 'NONE', *, *, #339, .F. ) ;
#9910 = ADVANCED_FACE ( 'NONE', ( #4770 ), #18150, .F. ) ;
#9911 = CARTESIAN_POINT ( 'NONE',  ( 13.54148016078094408, 12.79228088949424169, 5.988512446806296907 ) ) ;
#9912 = PRODUCT_RELATED_PRODUCT_CATEGORY ( 'part', '', ( #4914 ) ) ;
#9913 = FACE_OUTER_BOUND ( 'NONE', #19597, .T. ) ;
#9914 = DIRECTION ( 'NONE',  ( -0.9790635044817342925, 0.000000000000000000, 0.2035550397114870846 ) ) ;
#9915 = VECTOR ( 'NONE', #13345, 1000.000000000000000 ) ;
#9916 = FACE_OUTER_BOUND ( 'NONE', #7342, .T. ) ;
#9917 = CARTESIAN_POINT ( 'NONE',  ( 1.664752218687819862, 14.78848634200338452, -0.4464510495472899243 ) ) ;
#9918 = EDGE_CURVE ( 'NONE', #17422, #16118, #16860, .T. ) ;
#9919 = AXIS2_PLACEMENT_3D ( 'NONE', #6470, #4486, #4591 ) ;
#9920 = ORIENTED_EDGE ( 'NONE', *, *, #17505, .F. ) ;
#9921 = EDGE_CURVE ( 'NONE', #10689, #18275, #13187, .T. ) ;
#9922 = AXIS2_PLACEMENT_3D ( 'NONE', #17538, #9447, #19293 ) ;
#9923 = CARTESIAN_POINT ( 'NONE',  ( 70.64340948846358970, 32.54502000000000095, -10.53785647675949910 ) ) ;
#9924 = LINE ( 'NONE', #18643, #2558 ) ;
#9925 = CARTESIAN_POINT ( 'NONE',  ( 36.73521423675246922, 0.000000000000000000, 2.413462327205186497 ) ) ;
#9926 = LINE ( 'NONE', #3312, #19379 ) ;
#9927 = ORIENTED_EDGE ( 'NONE', *, *, #7682, .F. ) ;
#9928 = ORIENTED_EDGE ( 'NONE', *, *, #11297, .F. ) ;
#9929 = AXIS2_PLACEMENT_3D ( 'NONE', #1306, #11156, #19655 ) ;
#9930 = CARTESIAN_POINT ( 'NONE',  ( 10.60409020778431000, 11.65180524149912245, 3.905311891646460420 ) ) ;
#9932 = CARTESIAN_POINT ( 'NONE',  ( 46.03750000000000142, 34.52875999999999834, -10.31874999999999964 ) ) ;
#9931 = DIRECTION ( 'NONE',  ( 0.000000000000000000, 0.000000000000000000, -1.000000000000000000 ) ) ;
#9933 = EDGE_LOOP ( 'NONE', ( #17767, #21158, #12181, #7028 ) ) ;
#9934 = AXIS2_PLACEMENT_3D ( 'NONE', #12869, #16889, #4456 ) ;
#9935 = EDGE_LOOP ( 'NONE', ( #4552, #5 ) ) ;
#9936 = CARTESIAN_POINT ( 'NONE',  ( -21.73672411175306962, 32.54247999999999763, 0.8886449702404600748 ) ) ;
#9937 = ORIENTED_EDGE ( 'NONE', *, *, #2744, .F. ) ;
#9938 = CARTESIAN_POINT ( 'NONE',  ( 9.111805414026317607, 13.07579885469743708, 5.988343849954413933 ) ) ;
#9939 = CLOSED_SHELL ( 'NONE', ( #12314, #5130, #7289, #1659, #3174, #9118, #8286, #20285, #11694, #11427, #13760, #11105, #16019, #7338, #14895, #1385, #13612, #4395, #16804, #18856, #7266, #4247, #14005, #9860, #6322, #4350, #8994, #20983, #6542, #5085, #10806, #743, #6762, #18724, #15647, #13689, #13272, #8868, #4885, #1975, #14269, #15353, #17120, #13297, #3711, #1386, #15744, #6582, #3839, #2344, #19589, #18954, #4950, #1168, #10782, #2228, #19077, #11577, #21089, #6256, #9746, #7562, #9042, #9426, #14683, #16652, #5683, #7639, #9, #2343, #13738, #20157, #13121, #5767, #4764, #10448, #11929, #3819, #16598, #16415, #3323, #17116, #14973, #17373, #12736, #7607, #3074, #18577, #17477, #9910, #4514, #16779, #16407, #8122, #5063, #17523, #13221, #10073, #16307, #922, #15416, #5972 ) ) ;
#9940 = AXIS2_PLACEMENT_3D ( 'NONE', #8833, #3654, #18896 ) ;
#9941 = CIRCLE ( 'NONE', #4652, 0.7950199999999990608 ) ;
#9942 = ADVANCED_FACE ( 'NONE', ( #11502 ), #6535, .T. ) ;
#9943 = EDGE_CURVE ( 'NONE', #14493, #1074, #6623, .T. ) ;
#9944 = EDGE_CURVE ( 'NONE', #10623, #15859, #8292, .T. ) ;
#9945 = PLANE ( 'NONE',  #16594 ) ;
#9946 = PRESENTATION_LAYER_ASSIGNMENT (  '', '', ( #1491 ) ) ;
#9947 = CARTESIAN_POINT ( 'NONE',  ( 28.97711086133420366, 0.000000000000000000, -10.31874999999999964 ) ) ;
#9948 = CARTESIAN_POINT ( 'NONE',  ( 7.406270976683551055, 12.98268228153804138, 7.410819364758680194 ) ) ;
#9949 = CARTESIAN_POINT ( 'NONE',  ( -0.1146841969822216534, 16.89342109921696888, 0.05852849897634891663 ) ) ;
#9950 = CARTESIAN_POINT ( 'NONE',  ( 59.55063415577301811, 0.000000000000000000, -22.52230776719629191 ) ) ;
#9951 = VERTEX_POINT ( 'NONE', #3536 ) ;
#9952 = CARTESIAN_POINT ( 'NONE',  ( -0.01053909864879264136, 20.39392809349225999, 4.740337168719431560 ) ) ;
#9953 = CARTESIAN_POINT ( 'NONE',  ( 2.063750000000000195, 2.380615000000000148, 8.731249999999999289 ) ) ;
#9954 = LINE ( 'NONE', #16715, #7823 ) ;
#9955 = LINE ( 'NONE', #11733, #3614 ) ;
#9956 = PLANE ( 'NONE',  #9824 ) ;
#9957 = VECTOR ( 'NONE', #14275, 1000.000000000000000 ) ;
#9958 = ORIENTED_EDGE ( 'NONE', *, *, #13537, .F. ) ;
#9959 = AXIS2_PLACEMENT_3D ( 'NONE', #16998, #300, #7041 ) ;
#9960 = CARTESIAN_POINT ( 'NONE',  ( 9.693297870470777511, 21.84389315528099829, 3.625664949012268767 ) ) ;
#9961 = CARTESIAN_POINT ( 'NONE',  ( -0.1849527131266449076, 20.23672349358593792, 5.150944217628095068 ) ) ;
#9962 = CARTESIAN_POINT ( 'NONE',  ( 9.070785942620656073, 15.46259380661050464, -3.547234420078066996 ) ) ;
#9963 = ORIENTED_EDGE ( 'NONE', *, *, #7265, .T. ) ;
#9964 = VECTOR ( 'NONE', #1527, 1000.000000000000114 ) ;
#9965 = CARTESIAN_POINT ( 'NONE',  ( 7.550459306213158861, 21.69663300857961374, 3.242810284201234960 ) ) ;
#9966 = CIRCLE ( 'NONE', #19856, 0.3962400000000008138 ) ;
#9967 = CARTESIAN_POINT ( 'NONE',  ( -21.29909891687151813, -9.590920198756240467, -25.53841317587618320 ) ) ;
#9968 = DIRECTION ( 'NONE',  ( -0.6702301885068632226, 0.000000000000000000, -0.7421532822901576454 ) ) ;
#9969 = CARTESIAN_POINT ( 'NONE',  ( 6.218012969291997649, 20.30327552937278313, 5.288053756010064888 ) ) ;
#9970 = CARTESIAN_POINT ( 'NONE',  ( 30.25543876212147509, -1.983739999999999837, -19.39939755251907272 ) ) ;
#9971 = ORIENTED_EDGE ( 'NONE', *, *, #12382, .F. ) ;
#9972 = AXIS2_PLACEMENT_3D ( 'NONE', #15417, #244, #6982 ) ;
#9973 = EDGE_CURVE ( 'NONE', #16183, #2705, #8499, .T. ) ;
#9974 = CARTESIAN_POINT ( 'NONE',  ( 9.780308352758851242, 16.60610825764645071, 7.577664015808822207 ) ) ;
#9975 = CARTESIAN_POINT ( 'NONE',  ( 5.299730020803123942, 13.73299749091917121, 7.226549125627943937 ) ) ;
#9976 = CARTESIAN_POINT ( 'NONE',  ( 38.18512253410862201, -6.356984999999999886, -4.927479914652648674 ) ) ;
#9977 = CARTESIAN_POINT ( 'NONE',  ( 6.177406493418641453, 11.65935603284404287, 0.5479154027549586470 ) ) ;
#9978 = CYLINDRICAL_SURFACE ( 'NONE', #13913, 1.190624999999997824 ) ;
#9979 = VECTOR ( 'NONE', #1038, 1000.000000000000000 ) ;
#9980 = AXIS2_PLACEMENT_3D ( 'NONE', #17772, #10575, #11016 ) ;
#9981 = DIRECTION ( 'NONE',  ( 0.1060008583745199739, 0.000000000000000000, 0.9943660382494290406 ) ) ;
#9982 = CARTESIAN_POINT ( 'NONE',  ( 6.643788367457294619, 11.61924653269889163, 2.766513418718104855 ) ) ;
#9983 = CARTESIAN_POINT ( 'NONE',  ( 46.07940063401251507, -1.983739999999999837, -26.08707253294707229 ) ) ;
#9984 = CARTESIAN_POINT ( 'NONE',  ( 16.99218898555291446, -8.338783895011660618, -15.86074989063387264 ) ) ;
#9985 = LINE ( 'NONE', #14770, #12401 ) ;
#9986 = VERTEX_POINT ( 'NONE', #12272 ) ;
#9987 = DIRECTION ( 'NONE',  ( 0.000000000000000000, 1.000000000000000000, 0.000000000000000000 ) ) ;
#9988 = B_SPLINE_CURVE_WITH_KNOTS ( 'NONE', 3,
 ( #12899, #14443, #14341, #5907, #1042 ),
 .UNSPECIFIED., .F., .F.,
 ( 4, 1, 4 ),
 ( 0.007480389903054724364, 0.007494994329911808424, 0.007509598756768892484 ),
 .UNSPECIFIED. ) ;
#9989 = CARTESIAN_POINT ( 'NONE',  ( -16.07247711516169275, -5.309201820043501385, -10.44681224123558039 ) ) ;
#9990 = AXIS2_PLACEMENT_3D ( 'NONE', #10963, #15851, #12531 ) ;
#9991 = ORIENTED_EDGE ( 'NONE', *, *, #10605, .T. ) ;
#9992 = CARTESIAN_POINT ( 'NONE',  ( 13.13019290195440547, 16.36467473056671196, 6.416790074172170399 ) ) ;
#9993 = DIRECTION ( 'NONE',  ( 0.000000000000000000, -1.000000000000000000, 0.000000000000000000 ) ) ;
#9994 = CYLINDRICAL_SURFACE ( 'NONE', #17036, 6.349999999999997868 ) ;
#9995 = CARTESIAN_POINT ( 'NONE',  ( 11.51778461937661291, -4.547966530721023304, -15.27913115286716206 ) ) ;
#9997 = LINE ( 'NONE', #11447, #2163 ) ;
#9996 = CARTESIAN_POINT ( 'NONE',  ( 0.8190617032426232846, 18.54739417496245579, 8.495145815602461070 ) ) ;
#9998 = ORIENTED_EDGE ( 'NONE', *, *, #20311, .T. ) ;
#9999 = DIRECTION ( 'NONE',  ( 1.000000000000000000, 0.000000000000000000, 0.000000000000000000 ) ) ;
#10000 = DIRECTION ( 'NONE',  ( 0.9685006480810792739, 0.000000000000000000, 0.2490110332224846346 ) ) ;
#10001 = VERTEX_POINT ( 'NONE', #13504 ) ;
#10002 = VECTOR ( 'NONE', #10188, 1000.000000000000000 ) ;
#10003 = CARTESIAN_POINT ( 'NONE',  ( 6.039406833424090237, 11.15496817603752255, 2.913599363317485924 ) ) ;
#10004 = ADVANCED_FACE ( 'NONE', ( #15605 ), #1980, .F. ) ;
#10005 = ORIENTED_EDGE ( 'NONE', *, *, #7059, .T. ) ;
#10006 = CARTESIAN_POINT ( 'NONE',  ( 12.45327340276164740, 19.94235689841700321, 5.081717262054141315 ) ) ;
#10007 = AXIS2_PLACEMENT_3D ( 'NONE', #11311, #6444, #17953 ) ;
#10008 = CARTESIAN_POINT ( 'NONE',  ( 13.21401102953845275, 14.87494513186989664, 6.308780353949222430 ) ) ;
#10009 = FACE_OUTER_BOUND ( 'NONE', #2662, .T. ) ;
#10010 = CARTESIAN_POINT ( 'NONE',  ( 9.803413267150903110, 10.74905493727258232, 0.2107689867270556017 ) ) ;
#10011 = CARTESIAN_POINT ( 'NONE',  ( 17.25519468990899341, -7.034179569086526307, -15.81717762532307958 ) ) ;
#10012 = FILL_AREA_STYLE_COLOUR ( '', #18360 ) ;
#10013 = CIRCLE ( 'NONE', #488, 0.7950200000000003930 ) ;
#10014 = ORIENTED_EDGE ( 'NONE', *, *, #2395, .T. ) ;
#10015 = CARTESIAN_POINT ( 'NONE',  ( 8.719136823707652084, 20.76325780187099213, 0.7079147144396957803 ) ) ;
#10016 = CARTESIAN_POINT ( 'NONE',  ( 12.50377254232992108, 10.42934933986260049, 2.721148197543237668 ) ) ;
#10017 = CARTESIAN_POINT ( 'NONE',  ( 59.61686353177688602, 34.52875999999999834, -0.7993558564620834028 ) ) ;
#10018 = VERTEX_POINT ( 'NONE', #18892 ) ;
#10019 = ORIENTED_EDGE ( 'NONE', *, *, #9698, .F. ) ;
#10020 = CARTESIAN_POINT ( 'NONE',  ( 37.51913901087312553, -9.531985000000000596, -14.58057485080488114 ) ) ;
#10022 = DIRECTION ( 'NONE',  ( 0.000000000000000000, -1.000000000000000000, -0.000000000000000000 ) ) ;
#10021 = CARTESIAN_POINT ( 'NONE',  ( 0.7469844135213578040, 20.20533454244034033, 7.893868339785579558 ) ) ;
#10023 = ORIENTED_EDGE ( 'NONE', *, *, #13846, .T. ) ;
#10024 = CARTESIAN_POINT ( 'NONE',  ( 6.786416855358574196, 20.12019471844387652, 6.853687657227428787 ) ) ;
#10025 = VECTOR ( 'NONE', #5744, 1000.000000000000114 ) ;
#10026 = ORIENTED_EDGE ( 'NONE', *, *, #5863, .F. ) ;
#10027 = ORIENTED_EDGE ( 'NONE', *, *, #17287, .F. ) ;
#10028 = CARTESIAN_POINT ( 'NONE',  ( 0.1117406412582209324, 13.80476985362797748, 1.669220243459385022 ) ) ;
#10029 = ADVANCED_FACE ( 'NONE', ( #13723 ), #3429, .T. ) ;
#10030 = DIRECTION ( 'NONE',  ( -0.8943161143440100380, 0.000000000000000000, -0.4474356798743612806 ) ) ;
#10031 = EDGE_LOOP ( 'NONE', ( #6564, #3756, #13128, #1571 ) ) ;
#10032 = ADVANCED_FACE ( 'NONE', ( #5185 ), #12052, .F. ) ;
#10033 = TOROIDAL_SURFACE ( 'NONE', #12881, 3.174999999999999822, 0.5953125000000000222 ) ;
#10034 = CARTESIAN_POINT ( 'NONE',  ( 6.969492621012407518, 21.59576476661624156, 1.368388097798561631 ) ) ;
#10035 = CARTESIAN_POINT ( 'NONE',  ( 4.246403479487743660, 12.12027658721991052, 2.285455345423018869 ) ) ;
#10036 = DIRECTION ( 'NONE',  ( -0.000000000000000000, -1.000000000000000000, 0.000000000000000000 ) ) ;
#10037 = VECTOR ( 'NONE', #269, 1000.000000000000114 ) ;
#10038 = CARTESIAN_POINT ( 'NONE',  ( 39.37934099661365650, 40.07865999999999929, -4.303499184870370975 ) ) ;
#10039 = CARTESIAN_POINT ( 'NONE',  ( 1.669125073376063417, 14.66223945716840582, -0.4027805606639273117 ) ) ;
#10040 = ORIENTED_EDGE ( 'NONE', *, *, #11997, .F. ) ;
#10041 = DIRECTION ( 'NONE',  ( 0.6702301885068628895, 0.000000000000000000, 0.7421532822901579785 ) ) ;
#10042 = DIRECTION ( 'NONE',  ( 0.000000000000000000, 1.000000000000000000, 0.000000000000000000 ) ) ;
#10043 = PRESENTATION_STYLE_ASSIGNMENT (( #1852 ) ) ;
#10044 = PLANE ( 'NONE',  #19025 ) ;
#10045 = ORIENTED_EDGE ( 'NONE', *, *, #7163, .F. ) ;
#10046 = EDGE_LOOP ( 'NONE', ( #11495, #5090, #10969, #10123, #1421 ) ) ;
#10047 = CARTESIAN_POINT ( 'NONE',  ( 5.593306809071845187, 17.24227063501358614, -1.385594380044606000 ) ) ;
#10048 = CARTESIAN_POINT ( 'NONE',  ( -0.6905894489211669152, 20.80806006231328098, 3.719387543999512324 ) ) ;
#10049 = VECTOR ( 'NONE', #14325, 1000.000000000000227 ) ;
#10050 = VERTEX_POINT ( 'NONE', #17022 ) ;
#10051 = ADVANCED_FACE ( 'NONE', ( #106 ), #10499, .F. ) ;
#10052 = ORIENTED_EDGE ( 'NONE', *, *, #5945, .F. ) ;
#10053 = CARTESIAN_POINT ( 'NONE',  ( -160.2647810241784896, 30.16440499999999858, 8.335010000000000474 ) ) ;
#10054 = ORIENTED_EDGE ( 'NONE', *, *, #14354, .T. ) ;
#10055 = CARTESIAN_POINT ( 'NONE',  ( 8.854304133263051213, 12.09810837162069319, 4.755716881274997476 ) ) ;
#10056 = EDGE_CURVE ( 'NONE', #8805, #10374, #20316, .T. ) ;
#10057 = CARTESIAN_POINT ( 'NONE',  ( 3.299684148351696322, 17.13945079553905870, 8.374643251542508438 ) ) ;
#10058 = EDGE_CURVE ( 'NONE', #5959, #16695, #6856, .T. ) ;
#10059 = LINE ( 'NONE', #18563, #13218 ) ;
#10060 = CYLINDRICAL_SURFACE ( 'NONE', #521, 30.16250000000000142 ) ;
#10061 = CARTESIAN_POINT ( 'NONE',  ( -0.1842567146928706934, 14.65043659803843212, 0.3384235164672123597 ) ) ;
#10062 = ORIENTED_EDGE ( 'NONE', *, *, #15494, .T. ) ;
#10063 = CARTESIAN_POINT ( 'NONE',  ( 1.691847540349896484, 17.17955240639085801, 8.846950325066879728 ) ) ;
#10064 = CARTESIAN_POINT ( 'NONE',  ( 3.805353748838121053, -3.968114999999999615, -22.18284873352824960 ) ) ;
#10065 = CARTESIAN_POINT ( 'NONE',  ( 44.27024749654614055, -6.356984999999999886, -8.722764363618502159 ) ) ;
#10066 = DIRECTION ( 'NONE',  ( -0.2227372614607789347, 0.000000000000000000, -0.9748785115884710528 ) ) ;
#10067 = CARTESIAN_POINT ( 'NONE',  ( 10.72409186464205355, -4.809670885807086016, -15.96177715662992824 ) ) ;
#10068 = EDGE_LOOP ( 'NONE', ( #6910, #19538, #3152, #3390 ) ) ;
#10069 = CARTESIAN_POINT ( 'NONE',  ( 12.05093307044797690, 21.60877823626870153, -1.521190884665024390 ) ) ;
#10070 = CARTESIAN_POINT ( 'NONE',  ( 17.22522857595987844, -3.968114999999999615, -15.04442098945225403 ) ) ;
#10071 = CARTESIAN_POINT ( 'NONE',  ( 13.30764144135887861, 17.03292647117209668, 7.133305309152374818 ) ) ;
#10072 = EDGE_LOOP ( 'NONE', ( #5790, #16319, #7054, #16363 ) ) ;
#10073 = ADVANCED_FACE ( 'NONE', ( #8828, #13617, #7194, #13835, #1756 ), #8945, .T. ) ;
#10074 = EDGE_CURVE ( 'NONE', #9031, #16780, #2087, .T. ) ;
#10075 = EDGE_CURVE ( 'NONE', #14810, #7476, #11936, .T. ) ;
#10076 = CARTESIAN_POINT ( 'NONE',  ( 5.975876554808118968, 19.80119422045333621, -0.9882739879990679599 ) ) ;
#10077 = PLANE ( 'NONE',  #2809 ) ;
#10078 = CARTESIAN_POINT ( 'NONE',  ( 34.38097451710952868, -1.983739999999999837, 0.2081255904771098786 ) ) ;
#10079 = CARTESIAN_POINT ( 'NONE',  ( 12.11879977990919421, 20.23395749999999893, 0.1373704394269426865 ) ) ;
#10080 = CARTESIAN_POINT ( 'NONE',  ( 7.202655614464397615, 17.15635247398953922, 7.564427238666092457 ) ) ;
#10081 = DIRECTION ( 'NONE',  ( -0.2490110332224850231, 0.000000000000000000, 0.9685006480810791629 ) ) ;
#10082 = CIRCLE ( 'NONE', #5136, 30.16250000000000497 ) ;
#10083 = CARTESIAN_POINT ( 'NONE',  ( 10.72876945113536706, 10.85891277430018143, 2.065064361200644072 ) ) ;
#10084 = CARTESIAN_POINT ( 'NONE',  ( 5.338655627293653616, 14.14790490385028221, 7.478993364272384703 ) ) ;
#10085 = CARTESIAN_POINT ( 'NONE',  ( 1.272846674311993720, 18.94235087979956234, 8.991218144746445873 ) ) ;
#10086 = DIRECTION ( 'NONE',  ( 0.000000000000000000, -1.000000000000000000, 0.000000000000000000 ) ) ;
#10087 = DIRECTION ( 'NONE',  ( -0.2490110332224850231, 0.000000000000000000, 0.9685006480810791629 ) ) ;
#10088 = CARTESIAN_POINT ( 'NONE',  ( 3.114094397688433880, 12.59169734781732330, 6.492224364648873092 ) ) ;
#10089 = DIRECTION ( 'NONE',  ( -0.9129422336036122632, 0.000000000000000000, 0.4080888115384288528 ) ) ;
#10090 = CARTESIAN_POINT ( 'NONE',  ( 39.00487391863466513, 40.07742955315917044, -3.894748490060887747 ) ) ;
#10091 = CARTESIAN_POINT ( 'NONE',  ( 11.17185072860094763, -5.218912923018368843, -17.09259198936415913 ) ) ;
#10092 = CYLINDRICAL_SURFACE ( 'NONE', #16288, 0.5080000000000006732 ) ;
#10093 = ORIENTED_EDGE ( 'NONE', *, *, #13193, .T. ) ;
#10094 = CARTESIAN_POINT ( 'NONE',  ( 10.04743712810057765, 21.46699622675163255, 4.316190870212542663 ) ) ;
#10095 = CYLINDRICAL_SURFACE ( 'NONE', #21070, 0.7950200000000003930 ) ;
#10096 = VERTEX_POINT ( 'NONE', #5286 ) ;
#10097 = EDGE_CURVE ( 'NONE', #20863, #13842, #12168, .T. ) ;
#10098 = CARTESIAN_POINT ( 'NONE',  ( 13.15993927725578949, 14.64227085894461311, 6.133506565519140530 ) ) ;
#10099 = DIRECTION ( 'NONE',  ( 0.000000000000000000, 1.000000000000000000, 0.000000000000000000 ) ) ;
#10100 = CARTESIAN_POINT ( 'NONE',  ( 20.07182034886884381, -2.730729751928062665, -13.64168985034137549 ) ) ;
#10102 = DIRECTION ( 'NONE',  ( -0.2490110332224846623, 0.000000000000000000, 0.9685006480810793850 ) ) ;
#10101 = CARTESIAN_POINT ( 'NONE',  ( 3.630900445198600668, 12.75273057655540043, 0.9196498124107118644 ) ) ;
#10103 = ORIENTED_EDGE ( 'NONE', *, *, #16984, .F. ) ;
#10104 = CARTESIAN_POINT ( 'NONE',  ( -14.45909654372122688, -3.968114999999678538, -9.781826438796198175 ) ) ;
#10105 = CARTESIAN_POINT ( 'NONE',  ( 3.780468298635305313, 16.45009567437204723, -0.6686140809550422670 ) ) ;
#10106 = CARTESIAN_POINT ( 'NONE',  ( 6.107407430018315431, 11.04603590950089043, 2.885280809127467982 ) ) ;
#10107 = CARTESIAN_POINT ( 'NONE',  ( 20.39211608684103538, -6.633859764968358164, -15.26783537666067403 ) ) ;
#10108 = ORIENTED_EDGE ( 'NONE', *, *, #19385, .F. ) ;
#10109 = CARTESIAN_POINT ( 'NONE',  ( 9.098774907988232741, 21.15227197021270200, 1.770799497112857779 ) ) ;
#10110 = CARTESIAN_POINT ( 'NONE',  ( 3.956502030732897079, 20.47596928745859302, 4.905481943961070179 ) ) ;
#10111 = CARTESIAN_POINT ( 'NONE',  ( 7.855186243077828756, 12.04827940076156167, 0.2502000050339145965 ) ) ;
#10112 = FACE_OUTER_BOUND ( 'NONE', #13240, .T. ) ;
#10113 = CARTESIAN_POINT ( 'NONE',  ( 10.58862850081939300, 21.88976505986162024, 0.07107810111800938468 ) ) ;
#10114 = CARTESIAN_POINT ( 'NONE',  ( 11.98346169735263445, -2.082869424899609800, -16.75639176224798277 ) ) ;
#10115 = PRODUCT_DEFINITION_CONTEXT ( 'detailed design', #20907, 'design' ) ;
#10116 = DIRECTION ( 'NONE',  ( 0.000000000000000000, 1.000000000000000000, 0.000000000000000000 ) ) ;
#10117 = CIRCLE ( 'NONE', #4480, 1.190624999999997824 ) ;
#10118 = ORIENTED_EDGE ( 'NONE', *, *, #7614, .T. ) ;
#10119 = CARTESIAN_POINT ( 'NONE',  ( 10.74361481080007152, 19.05092171070422680, 6.014957688620392595 ) ) ;
#10120 = CARTESIAN_POINT ( 'NONE',  ( 10.93842014297040066, 16.27139374001615479, -4.478688491776773972 ) ) ;
#10121 = LINE ( 'NONE', #16867, #19129 ) ;
#10122 = ORIENTED_EDGE ( 'NONE', *, *, #10218, .F. ) ;
#10123 = ORIENTED_EDGE ( 'NONE', *, *, #5107, .F. ) ;
#10124 = EDGE_CURVE ( 'NONE', #4031, #10557, #5514, .T. ) ;
#10125 = DIRECTION ( 'NONE',  ( -0.9964481331860212121, 0.000000000000000000, 0.08420877549337302259 ) ) ;
#10126 = CARTESIAN_POINT ( 'NONE',  ( 11.02468627644401344, 17.30767747894585895, -4.286972664956881118 ) ) ;
#10128 = CARTESIAN_POINT ( 'NONE',  ( 28.87608719841374949, 2.770822500000000854, -15.73691681567849976 ) ) ;
#10127 = CARTESIAN_POINT ( 'NONE',  ( 1.509340951120249130, 13.07595850747188315, 0.5422609684877979230 ) ) ;
#10129 = ORIENTED_EDGE ( 'NONE', *, *, #20187, .F. ) ;
#10130 = CARTESIAN_POINT ( 'NONE',  ( 5.852858095612075928, 21.45851731444311383, 4.363222383076143629 ) ) ;
#10131 = ORIENTED_EDGE ( 'NONE', *, *, #2872, .T. ) ;
#10132 = AXIS2_PLACEMENT_3D ( 'NONE', #1952, #10581, #19083 ) ;
#10133 = CARTESIAN_POINT ( 'NONE',  ( 29.36887348155339694, 30.56064500123875050, 10.71562877576799977 ) ) ;
#10134 = VERTEX_POINT ( 'NONE', #2313 ) ;
#10135 = FACE_OUTER_BOUND ( 'NONE', #3085, .T. ) ;
#10136 = DIRECTION ( 'NONE',  ( 0.000000000000000000, 1.000000000000000000, 0.000000000000000000 ) ) ;
#10137 = LINE ( 'NONE', #8586, #3372 ) ;
#10138 = CARTESIAN_POINT ( 'NONE',  ( 1.693150899634930040, 14.15944726460652348, -0.2048692773969919834 ) ) ;
#10139 = ORIENTED_EDGE ( 'NONE', *, *, #16412, .F. ) ;
#10140 = DIRECTION ( 'NONE',  ( -0.2490110332224857170, 0.000000000000000000, 0.9685006480810790519 ) ) ;
#10141 = CARTESIAN_POINT ( 'NONE',  ( 30.33489826846160398, 1.984375000000000000, -2.417033907079745525 ) ) ;
#10142 = DIRECTION ( 'NONE',  ( 0.000000000000000000, 1.000000000000000000, 0.000000000000000000 ) ) ;
#10143 = DIRECTION ( 'NONE',  ( 0.3542738219355897056, 0.000000000000000000, 0.9351417320872542627 ) ) ;
#10145 = CARTESIAN_POINT ( 'NONE',  ( 19.79612130048327145, -2.801990398175632002, -14.19231935140637724 ) ) ;
#10144 = DIRECTION ( 'NONE',  ( 0.000000000000000000, -1.000000000000000000, 0.000000000000000000 ) ) ;
#10146 = VERTEX_POINT ( 'NONE', #6361 ) ;
#10147 = EDGE_LOOP ( 'NONE', ( #8710, #5760, #13724, #9144, #6572, #16477, #7524, #21350, #2880, #3250, #20102, #8061, #9611, #5279, #8804, #21456, #7951, #17568, #12644, #14913, #21389, #5498, #14826, #3060, #14045, #20376, #11389, #12503, #5392, #6839, #16154, #312, #9415, #838, #1283, #13343, #2544, #5837, #16247, #18081 ) ) ;
#10148 = EDGE_CURVE ( 'NONE', #11658, #8237, #9584, .T. ) ;
#10149 = CARTESIAN_POINT ( 'NONE',  ( 5.881368144132508746, 18.80106227311165767, -0.8182108359018045451 ) ) ;
#10150 = VECTOR ( 'NONE', #18034, 1000.000000000000000 ) ;
#10151 = CARTESIAN_POINT ( 'NONE',  ( 0.7843704457339527591, -1.594802499999999013, -23.55949434567611078 ) ) ;
#10152 = VERTEX_POINT ( 'NONE', #14692 ) ;
#10153 = ORIENTED_EDGE ( 'NONE', *, *, #5282, .T. ) ;
#10154 = CARTESIAN_POINT ( 'NONE',  ( -1.345424459097947834, 12.30439499999999953, 2.648158502653860324 ) ) ;
#10155 = ORIENTED_EDGE ( 'NONE', *, *, #18480, .F. ) ;
#10156 = CARTESIAN_POINT ( 'NONE',  ( 8.943100994816060023, 12.35671964186176197, 5.167251557440379450 ) ) ;
#10157 = DIRECTION ( 'NONE',  ( -0.08420877549337300871, 0.000000000000000000, -0.9964481331860212121 ) ) ;
#10158 = VECTOR ( 'NONE', #16063, 1000.000000000000000 ) ;
#10159 = EDGE_CURVE ( 'NONE', #6378, #5048, #16334, .T. ) ;
#10160 = CYLINDRICAL_SURFACE ( 'NONE', #7214, 1.190624999999999822 ) ;
#10161 = DIRECTION ( 'NONE',  ( 0.000000000000000000, -1.000000000000000000, 0.000000000000000000 ) ) ;
#10162 = CARTESIAN_POINT ( 'NONE',  ( 65.90927232300019512, -42.42568807200000691, -12.91110117861467899 ) ) ;
#10163 = CARTESIAN_POINT ( 'NONE',  ( 0.1527221624363179764, 18.60604061194695547, 0.5457984701511658931 ) ) ;
#10164 = CARTESIAN_POINT ( 'NONE',  ( -1.848761088705630051, 23.41816500000000190, 7.884515871828260636 ) ) ;
#10165 =( BOUNDED_CURVE ( )  B_SPLINE_CURVE ( 3, ( #17785, #2633, #9362, #16129 ),
 .UNSPECIFIED., .F., .T. ) 
 B_SPLINE_CURVE_WITH_KNOTS ( ( 4, 4 ),
 ( 4.712388980384104364, 5.524536188664038505 ),
 .UNSPECIFIED. ) 
 CURVE ( )  GEOMETRIC_REPRESENTATION_ITEM ( )  RATIONAL_B_SPLINE_CURVE ( ( 1.000000000000000000, 0.9457858982560934935, 0.9457858982560934935, 1.000000000000000000 ) ) 
 REPRESENTATION_ITEM ( '' )  );
#10166 = VERTEX_POINT ( 'NONE', #18976 ) ;
#10167 = CARTESIAN_POINT ( 'NONE',  ( 4.673487404147415702, 11.78541955647214046, 3.777201821681576810 ) ) ;
#10168 = DIRECTION ( 'NONE',  ( -0.9685006480810793850, 0.000000000000000000, -0.2490110332224846623 ) ) ;
#10169 = CARTESIAN_POINT ( 'NONE',  ( 52.59626903419218280, -5.404081211114977634, -17.22676038219739780 ) ) ;
#10170 = DIRECTION ( 'NONE',  ( 0.000000000000000000, 1.000000000000000000, 0.000000000000000000 ) ) ;
#10171 = VERTEX_POINT ( 'NONE', #15805 ) ;
#10172 = EDGE_CURVE ( 'NONE', #2822, #6097, #20976, .T. ) ;
#10173 = CARTESIAN_POINT ( 'NONE',  ( 8.744384562554335716, 11.57391542797248007, 5.551989790062823005 ) ) ;
#10174 = EDGE_CURVE ( 'NONE', #19683, #21868, #14150, .T. ) ;
#10175 = ADVANCED_FACE ( 'NONE', ( #9030 ), #1066, .T. ) ;
#10176 = CARTESIAN_POINT ( 'NONE',  ( 10.68696473053424967, 21.82883031116149297, 0.2667890350525887744 ) ) ;
#10177 = AXIS2_PLACEMENT_3D ( 'NONE', #11508, #4978, #3110 ) ;
#10178 = CARTESIAN_POINT ( 'NONE',  ( 9.350008301323910587, 12.97765481918709085, 6.896721531191268184 ) ) ;
#10179 = CARTESIAN_POINT ( 'NONE',  ( 7.309199775707146074, 16.58792154420486042, 7.713755225109836466 ) ) ;
#10180 = DIRECTION ( 'NONE',  ( 0.000000000000000000, 1.000000000000000000, 0.000000000000000000 ) ) ;
#10181 = PRODUCT_DEFINITION_FORMATION_WITH_SPECIFIED_SOURCE ( 'ANY', '', #19193, .NOT_KNOWN. ) ;
#10182 = CARTESIAN_POINT ( 'NONE',  ( 0.8373503019344407106, 19.61574039456632690, 2.335197277426223739 ) ) ;
#10183 = DIRECTION ( 'NONE',  ( 0.9579671649362032637, 0.000000000000000000, -0.2868778675745010664 ) ) ;
#10184 = CARTESIAN_POINT ( 'NONE',  ( 7.733788100231727469, 14.51543401643281150, -2.412536282348112238 ) ) ;
#10185 = EDGE_CURVE ( 'NONE', #5344, #1525, #9798, .T. ) ;
#10186 = CYLINDRICAL_SURFACE ( 'NONE', #6704, 9.524999999999998579 ) ;
#10187 = CARTESIAN_POINT ( 'NONE',  ( 7.367229612691850171, 18.51696245222963455, 8.037950014293697265 ) ) ;
#10188 = DIRECTION ( 'NONE',  ( 0.000000000000000000, 1.000000000000000000, 0.000000000000000000 ) ) ;
#10189 = AXIS2_PLACEMENT_3D ( 'NONE', #21654, #12950, #21759 ) ;
#10190 = CARTESIAN_POINT ( 'NONE',  ( 36.80301088673436283, 34.52875999999999834, -23.10021947667301134 ) ) ;
#10191 = CARTESIAN_POINT ( 'NONE',  ( 2.347314355769781091, 20.09598732912352403, 6.298940065843233072 ) ) ;
#10192 = CARTESIAN_POINT ( 'NONE',  ( -19.26432987443570966, 38.49878000000000355, -73.22178168742661342 ) ) ;
#10193 = CARTESIAN_POINT ( 'NONE',  ( 15.22903305875954594, -8.380302064858637934, -16.24791865429935100 ) ) ;
#10194 = CARTESIAN_POINT ( 'NONE',  ( 49.72033008250774344, 42.06303499999999929, -2.687827786179598277 ) ) ;
#10195 = ORIENTED_EDGE ( 'NONE', *, *, #20904, .F. ) ;
#10196 = CARTESIAN_POINT ( 'NONE',  ( 37.09580597189848561, 38.88803500000000213, 2.672127428255844261 ) ) ;
#10197 = EDGE_CURVE ( 'NONE', #4510, #6097, #21075, .T. ) ;
#10198 = CARTESIAN_POINT ( 'NONE',  ( 11.12927268506130929, 13.52938648361508100, 5.972454599576855649 ) ) ;
#10199 = CARTESIAN_POINT ( 'NONE',  ( 10.64684779959870298, 20.38904377012663716, 5.920590089696055713 ) ) ;
#10200 = DIRECTION ( 'NONE',  ( -0.9987059298363657467, 0.000000000000000000, -0.05085730733808409287 ) ) ;
#10201 = ORIENTED_EDGE ( 'NONE', *, *, #9143, .F. ) ;
#10202 = CARTESIAN_POINT ( 'NONE',  ( 12.53365458789522080, 11.46648469212541244, 3.032982017095954941 ) ) ;
#10203 = CARTESIAN_POINT ( 'NONE',  ( 12.36433962874629877, -0.5403542521652121566, -16.63866349071987827 ) ) ;
#10205 = CARTESIAN_POINT ( 'NONE',  ( 29.36874999999999858, 0.000000000000000000, 10.71562499999999929 ) ) ;
#10204 = CARTESIAN_POINT ( 'NONE',  ( 4.921664833983353304, 12.88680353640996223, 6.808023123837544155 ) ) ;
#10206 = VERTEX_POINT ( 'NONE', #2629 ) ;
#10207 =( NAMED_UNIT ( * ) SI_UNIT ( $, .STERADIAN. ) SOLID_ANGLE_UNIT ( ) );
#10208 = CARTESIAN_POINT ( 'NONE',  ( 3.805353748838121053, -3.968114999999999615, -22.18284873352824960 ) ) ;
#10209 = FACE_OUTER_BOUND ( 'NONE', #3477, .T. ) ;
#10210 = CIRCLE ( 'NONE', #680, 0.7950200000000000600 ) ;
#10211 = CARTESIAN_POINT ( 'NONE',  ( 6.113655373600792586, 11.03939097578738071, 2.882924309803769347 ) ) ;
#10212 = CIRCLE ( 'NONE', #9506, 1.983739999999995396 ) ;
#10213 = ORIENTED_EDGE ( 'NONE', *, *, #15360, .T. ) ;
#10214 = CARTESIAN_POINT ( 'NONE',  ( 11.11537376329170179, 14.44107328295670634, -3.331267459799296837 ) ) ;
#10215 = EDGE_CURVE ( 'NONE', #6097, #19275, #19414, .T. ) ;
#10216 = CARTESIAN_POINT ( 'NONE',  ( 10.13616474230335740, 20.26417264612534197, -1.207278885743884089 ) ) ;
#10217 = CARTESIAN_POINT ( 'NONE',  ( 2.299349580604229448, 13.27625335140768215, 0.5631475405237129639 ) ) ;
#10218 = EDGE_CURVE ( 'NONE', #19233, #14947, #6267, .T. ) ;
#10219 = CARTESIAN_POINT ( 'NONE',  ( 14.00687195125745887, 21.64281653910636294, 3.694034086410758366 ) ) ;
#10220 = CARTESIAN_POINT ( 'NONE',  ( 12.34662851096885916, -4.975191070769994006, -16.80281937503197298 ) ) ;
#10221 = CARTESIAN_POINT ( 'NONE',  ( 10.85253788098002836, -4.717387943497917568, -15.38032343689423875 ) ) ;
#10222 = ORIENTED_EDGE ( 'NONE', *, *, #6622, .T. ) ;
#10223 = CARTESIAN_POINT ( 'NONE',  ( 10.70179625483013730, 19.19642187053233329, 5.916294423283699366 ) ) ;
#10224 = CARTESIAN_POINT ( 'NONE',  ( 14.05130128282920232, 21.64220180175570363, 3.680409539941097208 ) ) ;
#10225 = ORIENTED_EDGE ( 'NONE', *, *, #20018, .F. ) ;
#10226 = EDGE_LOOP ( 'NONE', ( #21507, #18392, #19848, #10005 ) ) ;
#10227 = CARTESIAN_POINT ( 'NONE',  ( 28.87608719841374949, 2.770822500000000854, -15.73691681567849976 ) ) ;
#10228 = CARTESIAN_POINT ( 'NONE',  ( 12.85510060975789060, 22.16293208523041258, 0.4350888124966122428 ) ) ;
#10229 = AXIS2_PLACEMENT_3D ( 'NONE', #3001, #21022, #14405 ) ;
#10231 = DIRECTION ( 'NONE',  ( 3.502369222646484109E-14, 0.000000000000000000, 1.000000000000000000 ) ) ;
#10230 = CARTESIAN_POINT ( 'NONE',  ( 5.159230185404290125, 17.48971098885959918, 8.784928378633825474 ) ) ;
#10232 = VERTEX_POINT ( 'NONE', #7703 ) ;
#10233 = CARTESIAN_POINT ( 'NONE',  ( 7.245977530762245600, 18.46665735122999052, 7.961998677432508664 ) ) ;
#10234 = AXIS2_PLACEMENT_3D ( 'NONE', #290, #2370, #7031 ) ;
#10235 = ORIENTED_EDGE ( 'NONE', *, *, #14170, .F. ) ;
#10236 = VECTOR ( 'NONE', #12403, 1000.000000000000000 ) ;
#10237 = CARTESIAN_POINT ( 'NONE',  ( 32.42378190387104553, 32.54502000000000095, -18.15178106273469183 ) ) ;
#10238 = ORIENTED_EDGE ( 'NONE', *, *, #18355, .T. ) ;
#10239 = CARTESIAN_POINT ( 'NONE',  ( 2.042440755766480098, 13.25699772772027529, 1.354434111151779474 ) ) ;
#10240 = EDGE_CURVE ( 'NONE', #2714, #18576, #19203, .T. ) ;
#10241 = CARTESIAN_POINT ( 'NONE',  ( 3.828036625945912874, 13.64012675898730187, 0.2356414614424844622 ) ) ;
#10242 = VECTOR ( 'NONE', #3567, 1000.000000000000114 ) ;
#10243 = CYLINDRICAL_SURFACE ( 'NONE', #15658, 0.5079999999999996740 ) ;
#10244 = DIRECTION ( 'NONE',  ( 0.2868778675745010664, 0.000000000000000000, 0.9579671649362032637 ) ) ;
#10245 = LINE ( 'NONE', #10364, #2663 ) ;
#10246 = CARTESIAN_POINT ( 'NONE',  ( 1.666440852445509879, 15.73961440154546310, -0.6526140317216138076 ) ) ;
#10247 = CARTESIAN_POINT ( 'NONE',  ( 54.36523883999320361, 30.56064500000000095, -30.28170612544299800 ) ) ;
#10248 = ORIENTED_EDGE ( 'NONE', *, *, #11830, .F. ) ;
#10249 = DIRECTION ( 'NONE',  ( 0.000000000000000000, -1.000000000000000000, -0.000000000000000000 ) ) ;
#10250 = DIRECTION ( 'NONE',  ( 0.000000000000000000, 1.000000000000000000, 0.000000000000000000 ) ) ;
#10251 = FACE_BOUND ( 'NONE', #2465, .T. ) ;
#10253 = CARTESIAN_POINT ( 'NONE',  ( 13.84999724918104391, -6.798182784255816458, -15.30952765826574513 ) ) ;
#10252 = CARTESIAN_POINT ( 'NONE',  ( 3.360635606688116894, -1.983739999999999393, -20.45316710734507026 ) ) ;
#10254 = VERTEX_POINT ( 'NONE', #17558 ) ;
#10255 = ORIENTED_EDGE ( 'NONE', *, *, #18942, .F. ) ;
#10256 = CARTESIAN_POINT ( 'NONE',  ( 5.720661490769825441, 12.70293317459338134, 0.2232859597839690347 ) ) ;
#10258 = DIRECTION ( 'NONE',  ( -0.3140771401027084853, 0.9459569826691583971, -0.08075231887918270235 ) ) ;
#10257 = CARTESIAN_POINT ( 'NONE',  ( 7.159729259274372204, 11.65952799072720047, 5.998687542543657436 ) ) ;
#10259 = CIRCLE ( 'NONE', #13111, 0.3962400000000008138 ) ;
#10260 = ORIENTED_EDGE ( 'NONE', *, *, #16069, .T. ) ;
#10261 = ORIENTED_EDGE ( 'NONE', *, *, #5242, .T. ) ;
#10262 = CARTESIAN_POINT ( 'NONE',  ( 46.03750000000000142, -14.84248999999999974, -10.31874999999999964 ) ) ;
#10263 = ORIENTED_EDGE ( 'NONE', *, *, #2738, .F. ) ;
#10264 = VECTOR ( 'NONE', #2597, 1000.000000000000000 ) ;
#10265 = CARTESIAN_POINT ( 'NONE',  ( 7.468644793988906905, 14.27831657605653604, -1.663655224044803926 ) ) ;
#10266 = TOROIDAL_SURFACE ( 'NONE', #5323, 4.961572499999999941, 0.3962400000000000366 ) ;
#10267 = EDGE_CURVE ( 'NONE', #9142, #9809, #738, .T. ) ;
#10268 = CARTESIAN_POINT ( 'NONE',  ( 1.169308704210513694, -0.7997824999999986195, -20.81168733838920915 ) ) ;
#10269 = AXIS2_PLACEMENT_3D ( 'NONE', #14681, #6241, #13014 ) ;
#10270 = AXIS2_PLACEMENT_3D ( 'NONE', #6784, #8755, #13432 ) ;
#10271 = DIRECTION ( 'NONE',  ( 0.9987059298363657467, 0.000000000000000000, 0.05085730733808445370 ) ) ;
#10272 = CARTESIAN_POINT ( 'NONE',  ( -0.1334278631421785821, 13.87292853438413687, 0.7019017698175864517 ) ) ;
#10273 = DIRECTION ( 'NONE',  ( 0.000000000000000000, 0.000000000000000000, 1.000000000000000000 ) ) ;
#10274 = ORIENTED_EDGE ( 'NONE', *, *, #2620, .T. ) ;
#10275 = CARTESIAN_POINT ( 'NONE',  ( 3.141552985354155059, 11.94763405986570071, 5.008148756522596834 ) ) ;
#10276 = DIRECTION ( 'NONE',  ( -0.7421532822901562021, 0.000000000000000000, 0.6702301885068651099 ) ) ;
#10277 = DIRECTION ( 'NONE',  ( -0.9784543669157950152, 0.000000000000000000, -0.2064631973582961577 ) ) ;
#10278 = CARTESIAN_POINT ( 'NONE',  ( 45.99559936598748777, -1.983739999999999837, 5.449572532947073000 ) ) ;
#10279 = CARTESIAN_POINT ( 'NONE',  ( 41.78116128337411794, 0.000000000000000000, 7.392073290253172502 ) ) ;
#10280 = VERTEX_POINT ( 'NONE', #16126 ) ;
#10281 = CARTESIAN_POINT ( 'NONE',  ( 12.74908984681135138, 22.29005399844394120, 0.4156185081117323432 ) ) ;
#10282 = CARTESIAN_POINT ( 'NONE',  ( 26.41404040124396602, 0.001587500000000546807, -1.242873262350622010 ) ) ;
#10283 = CARTESIAN_POINT ( 'NONE',  ( 10.74838682008468638, 21.87703791083306371, 0.4363949013415037159 ) ) ;
#10284 = ORIENTED_EDGE ( 'NONE', *, *, #10498, .F. ) ;
#10285 = CIRCLE ( 'NONE', #3586, 22.02656249999999005 ) ;
#10286 = ORIENTED_EDGE ( 'NONE', *, *, #21101, .F. ) ;
#10287 = CIRCLE ( 'NONE', #11719, 0.3962399999999975386 ) ;
#10288 = VECTOR ( 'NONE', #4982, 1000.000000000000114 ) ;
#10289 = CARTESIAN_POINT ( 'NONE',  ( 9.073022245511658923, 11.70236418326780203, 5.603503291933394692 ) ) ;
#10290 = CARTESIAN_POINT ( 'NONE',  ( 5.642955815196034841, 20.83420574847494322, 3.727832798710557505 ) ) ;
#10291 = CARTESIAN_POINT ( 'NONE',  ( 2.520748753591570690, 102.1610225000000014, -24.56335908395234924 ) ) ;
#10292 = EDGE_CURVE ( 'NONE', #8259, #4430, #10705, .T. ) ;
#10293 = DIRECTION ( 'NONE',  ( 0.000000000000000000, -1.000000000000000000, 0.000000000000000000 ) ) ;
#10294 = CARTESIAN_POINT ( 'NONE',  ( 7.300217370997200028, 16.06868654239796257, 7.623995498661889414 ) ) ;
#10295 = VECTOR ( 'NONE', #2866, 1000.000000000000000 ) ;
#10296 = CARTESIAN_POINT ( 'NONE',  ( 1.860637697812923763, 20.38936078815874353, 4.959448130920145026 ) ) ;
#10297 = DIRECTION ( 'NONE',  ( -0.9784543669157947932, 0.000000000000000000, -0.2064631973582977953 ) ) ;
#10298 = ADVANCED_FACE ( 'NONE', ( #12690 ), #16234, .T. ) ;
#10299 =( BOUNDED_CURVE ( )  B_SPLINE_CURVE ( 3, ( #15106, #3148, #10104, #258 ),
 .UNSPECIFIED., .F., .F. ) 
 B_SPLINE_CURVE_WITH_KNOTS ( ( 4, 4 ),
 ( 0.7586491185162420603, 1.570796326795481868 ),
 .UNSPECIFIED. ) 
 CURVE ( )  GEOMETRIC_REPRESENTATION_ITEM ( )  RATIONAL_B_SPLINE_CURVE ( ( 1.000000000000000000, 0.9457858982561848649, 0.9457858982561848649, 1.000000000000000000 ) ) 
 REPRESENTATION_ITEM ( '' )  );
#10300 = CARTESIAN_POINT ( 'NONE',  ( 13.11534328330504451, 11.87357545845056173, 4.170984102655784120 ) ) ;
#10301 = EDGE_CURVE ( 'NONE', #11142, #14819, #14360, .T. ) ;
#10302 = AXIS2_PLACEMENT_3D ( 'NONE', #8264, #13691, #20076 ) ;
#10303 = CARTESIAN_POINT ( 'NONE',  ( 1.458975506666385424, 12.54422677008150089, 8.034613268192803304 ) ) ;
#10304 = DIRECTION ( 'NONE',  ( 0.7421532822901579785, -0.000000000000000000, -0.6702301885068630005 ) ) ;
#10305 = VECTOR ( 'NONE', #18329, 1000.000000000000000 ) ;
#10306 = AXIS2_PLACEMENT_3D ( 'NONE', #17696, #19663, #4530 ) ;
#10307 = DIRECTION ( 'NONE',  ( 0.000000000000000000, 1.000000000000000000, 0.000000000000000000 ) ) ;
#10308 = CARTESIAN_POINT ( 'NONE',  ( -0.3331096548604842722, 20.30753595452681992, 4.844414039309315356 ) ) ;
#10309 = CARTESIAN_POINT ( 'NONE',  ( 29.37324403177899868, 32.54502000000000095, -10.70578951775076071 ) ) ;
#10310 = CARTESIAN_POINT ( 'NONE',  ( 10.82835441204896298, -1.966650465303993567, -17.05962226904667389 ) ) ;
#10311 = CARTESIAN_POINT ( 'NONE',  ( 16.85197508397059707, 19.43957250000000059, -16.77951971243562923 ) ) ;
#10312 = CIRCLE ( 'NONE', #19479, 6.350000000000005862 ) ;
#10313 = VECTOR ( 'NONE', #17143, 1000.000000000000000 ) ;
#10314 = CARTESIAN_POINT ( 'NONE',  ( 11.42390536508826138, 16.05844251236355191, 7.572047171115840136 ) ) ;
#10315 = VERTEX_POINT ( 'NONE', #17781 ) ;
#10316 = CARTESIAN_POINT ( 'NONE',  ( 11.16572056210525865, 14.41814247312392183, -3.213472714937148478 ) ) ;
#10317 = CARTESIAN_POINT ( 'NONE',  ( 9.335363283976800375, -3.968114999999999615, -14.20581391854862474 ) ) ;
#10319 = CARTESIAN_POINT ( 'NONE',  ( 9.907371917564091746, 34.52875999999999834, -13.23786778167655243 ) ) ;
#10318 = CARTESIAN_POINT ( 'NONE',  ( 4.249450599936705153, 19.94879251081626137, 6.535985519458143322 ) ) ;
#10320 = VERTEX_POINT ( 'NONE', #5603 ) ;
#10321 = EDGE_CURVE ( 'NONE', #12395, #6616, #14465, .T. ) ;
#10322 = CARTESIAN_POINT ( 'NONE',  ( 17.22522857595987844, 34.52875999999999834, -15.04442098945225403 ) ) ;
#10323 = CIRCLE ( 'NONE', #8208, 3.770312499999998845 ) ;
#10324 = DIRECTION ( 'NONE',  ( 0.4128958666089267981, -0.5884034904305870395, -0.6951966166390379787 ) ) ;
#10325 = CARTESIAN_POINT ( 'NONE',  ( 6.273626380189087470, 10.93980219448746283, 2.827745728986147178 ) ) ;
#10326 = AXIS2_PLACEMENT_3D ( 'NONE', #3251, #11975, #15197 ) ;
#10327 = CARTESIAN_POINT ( 'NONE',  ( 20.07493000556766205, 0.4717600457865012142, -14.72462693936004285 ) ) ;
#10328 = ORIENTED_EDGE ( 'NONE', *, *, #16837, .F. ) ;
#10329 = CIRCLE ( 'NONE', #18437, 9.525000000000002132 ) ;
#10330 = CARTESIAN_POINT ( 'NONE',  ( 9.886766943894276238, 11.51584134576680363, 0.4567744769608155231 ) ) ;
#10331 = ADVANCED_FACE ( 'NONE', ( #15917 ), #12586, .T. ) ;
#10332 = CARTESIAN_POINT ( 'NONE',  ( 3.634673147523096226, 20.58079426707816850, 4.062413416603754435 ) ) ;
#10333 = CARTESIAN_POINT ( 'NONE',  ( 12.88900610377207734, 21.48306739246610420, 0.4890693659201348908 ) ) ;
#10334 = CARTESIAN_POINT ( 'NONE',  ( 6.344447095476780873, 11.93061510394686131, 0.6566749515117876745 ) ) ;
#10335 = CARTESIAN_POINT ( 'NONE',  ( 5.382695099851752651, 13.59057812530450171, -1.531598659755918135 ) ) ;
#10336 = DIRECTION ( 'NONE',  ( 0.9685006480810793850, 0.000000000000000000, 0.2490110332224846623 ) ) ;
#10337 = AXIS2_PLACEMENT_3D ( 'NONE', #975, #2651, #16473 ) ;
#10338 = EDGE_CURVE ( 'NONE', #14783, #1582, #268, .T. ) ;
#10339 = CARTESIAN_POINT ( 'NONE',  ( 15.99064506707870414, 1.097848371653701083, -15.45815286304121727 ) ) ;
#10340 = CARTESIAN_POINT ( 'NONE',  ( 39.11079947626275555, -1.983739999999999837, -27.65534212225540500 ) ) ;
#10341 = ORIENTED_EDGE ( 'NONE', *, *, #9773, .T. ) ;
#10342 = CARTESIAN_POINT ( 'NONE',  ( 10.80126525386333824, 10.89862672135422095, 4.169966205966027850 ) ) ;
#10343 = ORIENTED_EDGE ( 'NONE', *, *, #9268, .F. ) ;
#10344 = LINE ( 'NONE', #17089, #17276 ) ;
#10345 = CYLINDRICAL_SURFACE ( 'NONE', #17765, 0.7950200000000000600 ) ;
#10346 = VECTOR ( 'NONE', #11314, 1000.000000000000000 ) ;
#10348 = CARTESIAN_POINT ( 'NONE',  ( 55.33978576324753362, 32.54502000000000095, -23.05096232720518756 ) ) ;
#10347 = CARTESIAN_POINT ( 'NONE',  ( 0.4653477503899910994, 11.40353646073516103, 4.946780524725718386 ) ) ;
#10349 = ORIENTED_EDGE ( 'NONE', *, *, #15086, .T. ) ;
#10350 = CARTESIAN_POINT ( 'NONE',  ( 6.777766060880455967, 11.08767916761746086, 4.480892634214041159 ) ) ;
#10351 = EDGE_CURVE ( 'NONE', #6373, #9830, #10915, .T. ) ;
#10352 = EDGE_CURVE ( 'NONE', #16343, #8304, #21295, .T. ) ;
#10353 = FACE_OUTER_BOUND ( 'NONE', #564, .T. ) ;
#10354 = EDGE_CURVE ( 'NONE', #8651, #21849, #7346, .T. ) ;
#10355 = ORIENTED_EDGE ( 'NONE', *, *, #7883, .T. ) ;
#10356 = CARTESIAN_POINT ( 'NONE',  ( 0.3974967306201093176, 12.59494073688686555, 3.148956390786026294 ) ) ;
#10357 = CIRCLE ( 'NONE', #18129, 0.5080000000000012284 ) ;
#10358 = LINE ( 'NONE', #16878, #5412 ) ;
#10359 = ORIENTED_EDGE ( 'NONE', *, *, #5736, .T. ) ;
#10360 = CARTESIAN_POINT ( 'NONE',  ( 3.962427028851731148, 12.89365793399433180, 0.9426411514076304954 ) ) ;
#10361 = AXIS2_PLACEMENT_3D ( 'NONE', #11070, #17826, #1401 ) ;
#10362 = CARTESIAN_POINT ( 'NONE',  ( -0.6285274567219200081, 1.984375000000000000, 8.854636014509949860 ) ) ;
#10363 = DIRECTION ( 'NONE',  ( 0.000000000000000000, 1.000000000000000000, -0.000000000000000000 ) ) ;
#10364 = CARTESIAN_POINT ( 'NONE',  ( 12.62386444219163373, 13.08957250000000094, -17.86660850434754266 ) ) ;
#10365 = CARTESIAN_POINT ( 'NONE',  ( 3.414047624806694436, 21.33360473058343842, 3.465166473578813466 ) ) ;
#10366 = CARTESIAN_POINT ( 'NONE',  ( 59.55063415577301811, -1.983739999999999837, -22.52230776719629191 ) ) ;
#10367 = ORIENTED_EDGE ( 'NONE', *, *, #7778, .F. ) ;
#10368 = DIRECTION ( 'NONE',  ( 0.000000000000000000, 0.000000000000000000, -1.000000000000000000 ) ) ;
#10369 = LINE ( 'NONE', #414, #18089 ) ;
#10370 = DIRECTION ( 'NONE',  ( -0.000000000000000000, 1.000000000000000000, 0.000000000000000000 ) ) ;
#10372 = CARTESIAN_POINT ( 'NONE',  ( 16.69192786310252785, -7.118735165633143680, -14.71864076686690126 ) ) ;
#10371 = CARTESIAN_POINT ( 'NONE',  ( 46.03750000000000142, 32.54502000000000095, -10.31874999999999964 ) ) ;
#10373 = AXIS2_PLACEMENT_3D ( 'NONE', #902, #13184, #1324 ) ;
#10374 = VERTEX_POINT ( 'NONE', #11746 ) ;
#10375 = ORIENTED_EDGE ( 'NONE', *, *, #3726, .T. ) ;
#10376 = CARTESIAN_POINT ( 'NONE',  ( 9.814576312521648305, 11.51990282145384015, 0.4798283062359162687 ) ) ;
#10378 = CARTESIAN_POINT ( 'NONE',  ( 12.25799425556778388, -3.968114999999999615, 0.2069032437451798767 ) ) ;
#10377 = CARTESIAN_POINT ( 'NONE',  ( 0.3991529941856173380, 11.62559268301756177, 3.149969643310115419 ) ) ;
#10379 = ORIENTED_EDGE ( 'NONE', *, *, #10430, .F. ) ;
#10380 = CARTESIAN_POINT ( 'NONE',  ( 5.589289644602882134, 14.56010236266069136, 8.502823875585745483 ) ) ;
#10381 = B_SPLINE_CURVE_WITH_KNOTS ( 'NONE', 3,
 ( #7353, #15889, #12332, #12666 ),
 .UNSPECIFIED., .F., .F.,
 ( 4, 4 ),
 ( -7.968845587669719102E-05, 0.0005316928842662705084 ),
 .UNSPECIFIED. ) ;
#10382 = EDGE_LOOP ( 'NONE', ( #20615, #9485, #3746, #20326 ) ) ;
#10383 = ADVANCED_FACE ( 'NONE', ( #1887 ), #3667, .F. ) ;
#10384 = DIRECTION ( 'NONE',  ( 0.8943161143440100380, 0.000000000000000000, 0.4474356798743612806 ) ) ;
#10385 = ORIENTED_EDGE ( 'NONE', *, *, #16956, .T. ) ;
#10386 = AXIS2_PLACEMENT_3D ( 'NONE', #18889, #648, #8825 ) ;
#10387 = CARTESIAN_POINT ( 'NONE',  ( 7.457877451773216926, 16.00203316895927586, -2.111994508504527968 ) ) ;
#10388 = ORIENTED_EDGE ( 'NONE', *, *, #992, .T. ) ;
#10389 = VECTOR ( 'NONE', #7134, 1000.000000000000000 ) ;
#10390 = LINE ( 'NONE', #647, #10025 ) ;
#10391 = DIRECTION ( 'NONE',  ( -0.2868778675745010664, 0.000000000000000000, -0.9579671649362032637 ) ) ;
#10392 = CARTESIAN_POINT ( 'NONE',  ( 9.256853431388732290, 36.51313500000000545, -17.09316853730597074 ) ) ;
#10393 = CARTESIAN_POINT ( 'NONE',  ( 1.014578268522615012, 20.76321888266333104, 2.702579939252432784 ) ) ;
#10394 = CARTESIAN_POINT ( 'NONE',  ( 27.40895291499714403, 34.52875999999999834, -9.088367920799473865 ) ) ;
#10395 = ORIENTED_EDGE ( 'NONE', *, *, #10321, .F. ) ;
#10396 = CARTESIAN_POINT ( 'NONE',  ( 4.199552796348193340, 18.69182423982057273, -0.1726145848212380651 ) ) ;
#10397 = VECTOR ( 'NONE', #9644, 1000.000000000000114 ) ;
#10398 = DIRECTION ( 'NONE',  ( -0.2672484743474491942, 0.000000000000000000, -0.9636276526537419507 ) ) ;
#10399 = DIRECTION ( 'NONE',  ( -0.7421532822901579785, -0.000000000000000000, 0.6702301885068630005 ) ) ;
#10400 = CARTESIAN_POINT ( 'NONE',  ( 48.78323016782857735, 0.000000000000000000, -25.79158832643865651 ) ) ;
#10401 = EDGE_LOOP ( 'NONE', ( #5759, #8038 ) ) ;
#10402 = CARTESIAN_POINT ( 'NONE',  ( 5.378103913977471784, 12.14871438356658295, -0.1654852939330033190 ) ) ;
#10403 = CARTESIAN_POINT ( 'NONE',  ( 43.29176983217143260, -1.983739999999999837, 5.154088326438659884 ) ) ;
#10404 = CARTESIAN_POINT ( 'NONE',  ( 13.39275425437221401, 15.07885496629254440, 7.046569758826037422 ) ) ;
#10405 = EDGE_LOOP ( 'NONE', ( #7083, #17250, #16868, #404 ) ) ;
#10406 = VECTOR ( 'NONE', #5402, 1000.000000000000000 ) ;
#10407 = CYLINDRICAL_SURFACE ( 'NONE', #3891, 9.524999999999998579 ) ;
#10408 = ORIENTED_EDGE ( 'NONE', *, *, #12589, .T. ) ;
#10409 = EDGE_CURVE ( 'NONE', #11247, #10898, #16725, .T. ) ;
#10410 = FACE_OUTER_BOUND ( 'NONE', #13168, .T. ) ;
#10411 = CARTESIAN_POINT ( 'NONE',  ( 9.037210512593977896, 11.60002287198769189, 5.445748904208223884 ) ) ;
#10412 = CARTESIAN_POINT ( 'NONE',  ( 3.728962736874319006, 15.57283695825947412, -0.6908591606584689737 ) ) ;
#10413 = DIRECTION ( 'NONE',  ( 0.000000000000000000, -1.000000000000000000, 0.000000000000000000 ) ) ;
#10414 = CARTESIAN_POINT ( 'NONE',  ( 5.706220423065773595, 17.18812784857371767, -1.328853644864197658 ) ) ;
#10415 = FACE_OUTER_BOUND ( 'NONE', #9360, .T. ) ;
#10416 = FACE_OUTER_BOUND ( 'NONE', #19945, .T. ) ;
#10417 = CARTESIAN_POINT ( 'NONE',  ( 9.747861764205893564, 16.62671289803297370, 7.918352333577308499 ) ) ;
#10418 = CARTESIAN_POINT ( 'NONE',  ( 5.132107606870269123, 12.79243504847817547, 6.338296502348789829 ) ) ;
#10419 = CIRCLE ( 'NONE', #14709, 30.16249999999999076 ) ;
#10420 = CARTESIAN_POINT ( 'NONE',  ( 5.244116213687740391, 19.21739139815786146, 8.049907794713583087 ) ) ;
#10421 = CARTESIAN_POINT ( 'NONE',  ( -29.36874999999999858, 30.16440499999999858, 8.335010000000000474 ) ) ;
#10422 = CARTESIAN_POINT ( 'NONE',  ( 20.23867309534036707, -1.248700931907035239, -14.75477345577187371 ) ) ;
#10423 = CARTESIAN_POINT ( 'NONE',  ( 0.6723359852304844342, 19.54979116365418079, 7.412813188025597633 ) ) ;
#10424 = LINE ( 'NONE', #13321, #11309 ) ;
#10425 = DIRECTION ( 'NONE',  ( 0.07875956036501312318, 0.000000000000000000, -0.9968936410927243807 ) ) ;
#10426 = CARTESIAN_POINT ( 'NONE',  ( 50.29383871662588490, 29.95901653600000003, -28.02957329025317179 ) ) ;
#10427 = CARTESIAN_POINT ( 'NONE',  ( 11.10489018155983310, 18.77048838114807694, 7.052920197992054163 ) ) ;
#10428 = DIRECTION ( 'NONE',  ( 1.000000000000000000, 0.000000000000000000, 0.000000000000000000 ) ) ;
#10429 = DIRECTION ( 'NONE',  ( -0.9161599507719021540, -0.3242921320961419940, -0.2355537256384720723 ) ) ;
#10430 = EDGE_CURVE ( 'NONE', #17367, #4043, #15512, .T. ) ;
#10431 = CARTESIAN_POINT ( 'NONE',  ( 11.24411629099876109, 17.10760633503948824, -3.541267089923193279 ) ) ;
#10432 = EDGE_CURVE ( 'NONE', #3770, #7380, #10530, .T. ) ;
#10433 = LINE ( 'NONE', #15534, #673 ) ;
#10435 = DIRECTION ( 'NONE',  ( 0.000000000000000000, 1.000000000000000000, 0.000000000000000000 ) ) ;
#10434 = CARTESIAN_POINT ( 'NONE',  ( 4.683303992135119387, 18.80848272075206040, 7.590210397258200459 ) ) ;
#10436 = VERTEX_POINT ( 'NONE', #232 ) ;
#10437 = PRODUCT_CONTEXT ( 'NONE', #10749, 'mechanical' ) ;
#10438 = VECTOR ( 'NONE', #2929, 1000.000000000000000 ) ;
#10439 = CARTESIAN_POINT ( 'NONE',  ( 0.1129727359843346046, 20.94457815707821169, 5.061725698818384522 ) ) ;
#10440 = CARTESIAN_POINT ( 'NONE',  ( 71.04062499999999147, 0.000000000000000000, -10.31874999999999964 ) ) ;
#10441 = CARTESIAN_POINT ( 'NONE',  ( 6.359934862478964668, 11.71523234649916212, 2.858519856524831315 ) ) ;
#10442 = ORIENTED_EDGE ( 'NONE', *, *, #2744, .T. ) ;
#10443 = CARTESIAN_POINT ( 'NONE',  ( 11.18095383545338528, 17.51254433608867700, 6.751878116475301006 ) ) ;
#10444 = CARTESIAN_POINT ( 'NONE',  ( 14.12523555123927999, 20.59139265233172367, 3.828121585696277140 ) ) ;
#10445 = CARTESIAN_POINT ( 'NONE',  ( 1.119724371970266974, 20.13149037663900387, 7.725538715806275825 ) ) ;
#10446 = CARTESIAN_POINT ( 'NONE',  ( 8.603371928060651541, 10.74414689430484238, 3.699663666938896256 ) ) ;
#10447 = DIRECTION ( 'NONE',  ( 0.9959941601142464629, 0.000000000000000000, 0.08941830359784717908 ) ) ;
#10448 = ADVANCED_FACE ( 'NONE', ( #13406 ), #5306, .T. ) ;
#10449 = CARTESIAN_POINT ( 'NONE',  ( 18.00500580558605890, 0.4330974563432516966, -14.83538992815904400 ) ) ;
#10450 = CARTESIAN_POINT ( 'NONE',  ( -53.00154558624916490, -5.714999999999999858, -22.85927301266823264 ) ) ;
#10451 = EDGE_LOOP ( 'NONE', ( #2321, #21768, #14071 ) ) ;
#10452 = CARTESIAN_POINT ( 'NONE',  ( 11.19102542510228382, 12.02330533696836135, 5.866022334646728176 ) ) ;
#10453 = EDGE_LOOP ( 'NONE', ( #5935, #10594, #16798, #16136 ) ) ;
#10454 = ADVANCED_FACE ( 'NONE', ( #3346 ), #3463, .T. ) ;
#10455 = CARTESIAN_POINT ( 'NONE',  ( 10.30239665667997251, 11.37017134450840139, 2.174391373805977690 ) ) ;
#10456 = DIRECTION ( 'NONE',  ( 0.2868778675745011220, 0.000000000000000000, 0.9579671649362034858 ) ) ;
#10457 = LINE ( 'NONE', #508, #14950 ) ;
#10458 = EDGE_CURVE ( 'NONE', #5796, #18904, #5584, .T. ) ;
#10460 = DIRECTION ( 'NONE',  ( 0.9579671649362032637, 0.000000000000000000, -0.2868778675745010664 ) ) ;
#10459 = CARTESIAN_POINT ( 'NONE',  ( 6.954974101898393712, 18.47894807998623534, 8.074325918837109484 ) ) ;
#10461 = ORIENTED_EDGE ( 'NONE', *, *, #18858, .F. ) ;
#10462 = CARTESIAN_POINT ( 'NONE',  ( -28.19602381335591801, -6.905625000000000568, -72.46697370030818774 ) ) ;
#10463 = VERTEX_POINT ( 'NONE', #10078 ) ;
#10464 = DIRECTION ( 'NONE',  ( -0.2490110332224857170, 0.000000000000000000, 0.9685006480810790519 ) ) ;
#10465 = VERTEX_POINT ( 'NONE', #11954 ) ;
#10466 = DIRECTION ( 'NONE',  ( -0.8943161143440100380, 0.000000000000000000, -0.4474356798743612806 ) ) ;
#10467 = CARTESIAN_POINT ( 'NONE',  ( 12.62386444219163373, 19.43957250000000059, -17.86660850434754266 ) ) ;
#10468 = ADVANCED_FACE ( 'NONE', ( #20330 ), #3445, .T. ) ;
#10469 = DIRECTION ( 'NONE',  ( -0.7532174416907910786, 0.000000000000000000, -0.6577716059034319773 ) ) ;
#10470 = PLANE ( 'NONE',  #9437 ) ;
#10471 = EDGE_CURVE ( 'NONE', #13225, #13907, #17595, .T. ) ;
#10472 = ORIENTED_EDGE ( 'NONE', *, *, #11011, .T. ) ;
#10473 = DIRECTION ( 'NONE',  ( 1.000000000000000000, 0.000000000000000000, 0.000000000000000000 ) ) ;
#10474 = CARTESIAN_POINT ( 'NONE',  ( 29.98909767165928386, 23.40768749999999798, -5.214162619065493054 ) ) ;
#10475 = CARTESIAN_POINT ( 'NONE',  ( 52.44708915697334106, 0.000000000000000000, 4.020247972991190188 ) ) ;
#10476 = CARTESIAN_POINT ( 'NONE',  ( 67.79270099634359781, 32.54502000000000095, -13.76558698117381851 ) ) ;
#10478 = CARTESIAN_POINT ( 'NONE',  ( 16.92682437108570426, -7.051316376102997552, -14.66989665197142578 ) ) ;
#10477 = CARTESIAN_POINT ( 'NONE',  ( 5.447351731530780228, 0.000000000000000000, 0.8930339070797439494 ) ) ;
#10479 = VERTEX_POINT ( 'NONE', #20230 ) ;
#10480 = VERTEX_POINT ( 'NONE', #12071 ) ;
#10481 = CARTESIAN_POINT ( 'NONE',  ( 12.37983225623493411, 19.93927778675710272, 5.100595263939720958 ) ) ;
#10483 = DIRECTION ( 'NONE',  ( 0.000000000000000000, -1.000000000000000000, -0.000000000000000000 ) ) ;
#10482 = CARTESIAN_POINT ( 'NONE',  ( -0.6995384825569825882, 20.80871142581116118, 3.721840415571334049 ) ) ;
#10484 = ORIENTED_EDGE ( 'NONE', *, *, #4141, .F. ) ;
#10486 = CARTESIAN_POINT ( 'NONE',  ( 17.55130215754536493, -8.551187338024273998, -15.76935921083538084 ) ) ;
#10485 = CARTESIAN_POINT ( 'NONE',  ( 4.551862264357088961, 11.07955752190297183, 3.668119238956743633 ) ) ;
#10487 = ORIENTED_EDGE ( 'NONE', *, *, #6375, .T. ) ;
#10488 = VECTOR ( 'NONE', #5012, 1000.000000000000000 ) ;
#10489 = ORIENTED_EDGE ( 'NONE', *, *, #18409, .F. ) ;
#10490 = CARTESIAN_POINT ( 'NONE',  ( 7.545096913039198938, 17.11720444957493825, -2.078483839830497004 ) ) ;
#10491 = VERTEX_POINT ( 'NONE', #5103 ) ;
#10492 = CARTESIAN_POINT ( 'NONE',  ( 29.98909767165928386, 30.50833916023545811, -5.214162619065493054 ) ) ;
#10493 = EDGE_CURVE ( 'NONE', #12681, #6123, #17155, .T. ) ;
#10494 = CARTESIAN_POINT ( 'NONE',  ( 62.90077106633562209, -3.968114999999999615, 8.141649473166729933 ) ) ;
#10495 = CARTESIAN_POINT ( 'NONE',  ( 1.597882609860227454, 23.48611691159180381, 8.700201306427871373 ) ) ;
#10496 = LINE ( 'NONE', #16905, #10406 ) ;
#10497 = CARTESIAN_POINT ( 'NONE',  ( 0.8685919227001404064, 20.56010016465687684, 2.317533322938851281 ) ) ;
#10498 = EDGE_CURVE ( 'NONE', #10232, #12825, #8403, .T. ) ;
#10499 = CYLINDRICAL_SURFACE ( 'NONE', #1323, 0.5079999999999996740 ) ;
#10500 = VECTOR ( 'NONE', #7806, 1000.000000000000000 ) ;
#10501 = ORIENTED_EDGE ( 'NONE', *, *, #2002, .F. ) ;
#10502 = CARTESIAN_POINT ( 'NONE',  ( 1.698299366653992282, 20.72409300549792022, 3.290495829865351940 ) ) ;
#10503 = CYLINDRICAL_SURFACE ( 'NONE', #16651, 0.7950199999999971734 ) ;
#10504 = CARTESIAN_POINT ( 'NONE',  ( 52.25302947726946456, -6.201940431049069780, -17.53628547414362515 ) ) ;
#10505 = CARTESIAN_POINT ( 'NONE',  ( 32.10373694497760511, -6.356984999999999886, -3.785462747693984831 ) ) ;
#10506 = EDGE_LOOP ( 'NONE', ( #21853, #19178, #16864, #9788 ) ) ;
#10507 = CARTESIAN_POINT ( 'NONE',  ( 10.32489209301978583, 21.80709644552430149, 0.1772959725815080045 ) ) ;
#10508 = CARTESIAN_POINT ( 'NONE',  ( 54.61912012054379062, -6.356984999999999886, -13.79062155615056362 ) ) ;
#10509 = CARTESIAN_POINT ( 'NONE',  ( 12.18859454906908546, 21.32141368478257348, 4.415751409964100205 ) ) ;
#10510 = ORIENTED_EDGE ( 'NONE', *, *, #979, .F. ) ;
#10511 = VERTEX_POINT ( 'NONE', #15410 ) ;
#10512 = CARTESIAN_POINT ( 'NONE',  ( 9.486764370443642846, 15.75061937992353123, 7.955153629647191416 ) ) ;
#10513 = CARTESIAN_POINT ( 'NONE',  ( 3.846219661981610471, 17.18860055147588994, -0.6938403426090347104 ) ) ;
#10514 = CARTESIAN_POINT ( 'NONE',  ( 18.65312499999999929, 32.54502000000000095, 5.159374999999999822 ) ) ;
#10515 = CARTESIAN_POINT ( 'NONE',  ( 5.782398285543762562, 12.98564521233307190, 0.02530286594647560006 ) ) ;
#10516 = CARTESIAN_POINT ( 'NONE',  ( 1.315381686729747646, 20.24764554913870995, 3.544931371820004173 ) ) ;
#10517 = CARTESIAN_POINT ( 'NONE',  ( 38.98667580346275940, 40.07845397843726687, -3.914708526915718689 ) ) ;
#10518 = CARTESIAN_POINT ( 'NONE',  ( 8.168165464054217395, 20.04452402401122058, -1.696596079913171851 ) ) ;
#10519 = LINE ( 'NONE', #2339, #9310 ) ;
#10520 = CARTESIAN_POINT ( 'NONE',  ( -12.21686131739395798, 0.000000000000000000, -1.090609736204202429 ) ) ;
#10521 = CARTESIAN_POINT ( 'NONE',  ( 6.940486874547567631, 20.09752422452572418, 7.007469641995731635 ) ) ;
#10522 = CARTESIAN_POINT ( 'NONE',  ( 1.255123740014034706, 18.92571547447176172, 8.878479688366162748 ) ) ;
#10523 = EDGE_CURVE ( 'NONE', #13662, #1981, #6972, .T. ) ;
#10524 = CARTESIAN_POINT ( 'NONE',  ( 67.79270099634359781, 0.000000000000000000, -13.76558698117381851 ) ) ;
#10525 = CARTESIAN_POINT ( 'NONE',  ( 1.297850727783172786, 13.15556036664986195, 7.528907847599255909 ) ) ;
#10526 = FACE_OUTER_BOUND ( 'NONE', #5613, .T. ) ;
#10527 = DIRECTION ( 'NONE',  ( 0.9237641507921645623, 0.000000000000000000, 0.3829618697876213673 ) ) ;
#10528 = CARTESIAN_POINT ( 'NONE',  ( 18.53801154572697385, 1.494989082069840824, -14.70250965503444540 ) ) ;
#10529 = DIRECTION ( 'NONE',  ( -0.7421532822901572013, 0.000000000000000000, 0.6702301885068637777 ) ) ;
#10530 = CIRCLE ( 'NONE', #11931, 0.5080000000000001181 ) ;
#10531 = FACE_OUTER_BOUND ( 'NONE', #9770, .T. ) ;
#10532 = CARTESIAN_POINT ( 'NONE',  ( 9.221657793164913741, 21.87308296202409963, 2.042460036653409805 ) ) ;
#10533 = LINE ( 'NONE', #14210, #407 ) ;
#10534 = CARTESIAN_POINT ( 'NONE',  ( 11.34677053555899029, 17.89547928321977466, -3.372900898699195071 ) ) ;
#10535 = CARTESIAN_POINT ( 'NONE',  ( -21.34815828341188393, 32.54247999999999763, 0.8078590638549643099 ) ) ;
#10536 = CARTESIAN_POINT ( 'NONE',  ( 6.384643824615721996, 11.62550227300026151, 4.197152387170460131 ) ) ;
#10537 = ORIENTED_EDGE ( 'NONE', *, *, #11086, .F. ) ;
#10538 = ITEM_DEFINED_TRANSFORMATION ( 'NONE', 'NONE', #9105,  #2234 ) ;
#10539 =( LENGTH_UNIT ( ) NAMED_UNIT ( * ) SI_UNIT ( .MILLI., .METRE. ) );
#10540 = CARTESIAN_POINT ( 'NONE',  ( 4.351297120991392653, 19.36269373579626674, 0.4388914768103922559 ) ) ;
#10541 = CARTESIAN_POINT ( 'NONE',  ( 64.66604708500285881, 32.54502000000000095, -11.54913207920052720 ) ) ;
#10542 = AXIS2_PLACEMENT_3D ( 'NONE', #18469, #555, #7075 ) ;
#10543 = VERTEX_POINT ( 'NONE', #568 ) ;
#10544 = CARTESIAN_POINT ( 'NONE',  ( 9.995376944861977364, 11.51990282145384015, 0.4256848013639417672 ) ) ;
#10545 = CARTESIAN_POINT ( 'NONE',  ( 9.360757232110890058, 13.73189003748300685, -2.250780131576506360 ) ) ;
#10546 = CARTESIAN_POINT ( 'NONE',  ( 6.054335174399104957, 21.23839086782724195, 3.633263926537354749 ) ) ;
#10547 = DIRECTION ( 'NONE',  ( 0.000000000000000000, -1.000000000000000000, 0.000000000000000000 ) ) ;
#10548 = ADVANCED_FACE ( 'NONE', ( #17489, #2223 ), #4106, .T. ) ;
#10549 = DIRECTION ( 'NONE',  ( 0.000000000000000000, -1.000000000000000000, 0.000000000000000000 ) ) ;
#10550 = VECTOR ( 'NONE', #11093, 1000.000000000000000 ) ;
#10551 = CARTESIAN_POINT ( 'NONE',  ( 18.91132178901277072, -0.4204008045333961219, -14.54213590646165422 ) ) ;
#10552 = PRODUCT_DEFINITION_CONTEXT ( 'detailed design', #6216, 'design' ) ;
#10553 = CARTESIAN_POINT ( 'NONE',  ( 10.97846818458738127, -4.667157448163489875, -15.28170016135478804 ) ) ;
#10554 = ORIENTED_EDGE ( 'NONE', *, *, #1060, .T. ) ;
#10555 = CARTESIAN_POINT ( 'NONE',  ( 12.15973251502179231, 21.60500416633145804, -1.551647953943186886 ) ) ;
#10556 = DIRECTION ( 'NONE',  ( 0.9636276526537417286, 0.000000000000000000, -0.2672484743474500268 ) ) ;
#10557 = VERTEX_POINT ( 'NONE', #464 ) ;
#10558 = CARTESIAN_POINT ( 'NONE',  ( 9.842819086504725590, 11.73374667394938164, 0.1685169991754134899 ) ) ;
#10559 = AXIS2_PLACEMENT_3D ( 'NONE', #5951, #4428, #12508 ) ;
#10560 = DIRECTION ( 'NONE',  ( 0.9579671649362033747, 0.000000000000000000, -0.2868778675745006779 ) ) ;
#10561 = CARTESIAN_POINT ( 'NONE',  ( 13.12625987927192739, 22.21723794295526488, 1.191615484091907762 ) ) ;
#10563 = CARTESIAN_POINT ( 'NONE',  ( -17.46249999999999858, 0.000000000000000000, 0.000000000000000000 ) ) ;
#10562 = CARTESIAN_POINT ( 'NONE',  ( -0.3645692649321460310, 17.35729252269350553, 0.2027727071106186774 ) ) ;
#10564 = VERTEX_POINT ( 'NONE', #19015 ) ;
#10565 = CARTESIAN_POINT ( 'NONE',  ( 7.400268487603801404, 13.00719617420639551, 7.282345073165821248 ) ) ;
#10566 = DIRECTION ( 'NONE',  ( 0.000000000000000000, -1.000000000000000000, 0.000000000000000000 ) ) ;
#10567 = VECTOR ( 'NONE', #13142, 1000.000000000000114 ) ;
#10568 = VERTEX_POINT ( 'NONE', #7212 ) ;
#10569 = FACE_OUTER_BOUND ( 'NONE', #8145, .T. ) ;
#10570 = EDGE_CURVE ( 'NONE', #12696, #14357, #20385, .T. ) ;
#10571 = CARTESIAN_POINT ( 'NONE',  ( 0.04787801191089360864, 14.49629642778351268, 1.235535862485549030 ) ) ;
#10572 = AXIS2_PLACEMENT_3D ( 'NONE', #18476, #16405, #11419 ) ;
#10573 = DIRECTION ( 'NONE',  ( 0.000000000000000000, -1.000000000000000000, 0.000000000000000000 ) ) ;
#10574 = ORIENTED_EDGE ( 'NONE', *, *, #14699, .F. ) ;
#10575 = DIRECTION ( 'NONE',  ( -0.7421532822901579785, 0.000000000000000000, 0.6702301885068630005 ) ) ;
#10576 = ADVANCED_FACE ( 'NONE', ( #3890 ), #2446, .T. ) ;
#10577 = EDGE_CURVE ( 'NONE', #18381, #21183, #1785, .T. ) ;
#10578 = EDGE_CURVE ( 'NONE', #16397, #16186, #19346, .T. ) ;
#10579 = DIRECTION ( 'NONE',  ( -0.000000000000000000, -1.000000000000000000, 0.000000000000000000 ) ) ;
#10580 = CARTESIAN_POINT ( 'NONE',  ( 32.16428892652708527, -6.356984999999999886, -4.974546995406843308 ) ) ;
#10581 = DIRECTION ( 'NONE',  ( 0.2490110332224850509, 0.000000000000000000, -0.9685006480810792739 ) ) ;
#10582 = EDGE_LOOP ( 'NONE', ( #4506, #16127, #18334, #18219 ) ) ;
#10583 = AXIS2_PLACEMENT_3D ( 'NONE', #2052, #10136, #11908 ) ;
#10584 = DIRECTION ( 'NONE',  ( 0.7421532822901579785, 0.000000000000000000, -0.6702301885068628895 ) ) ;
#10585 = CARTESIAN_POINT ( 'NONE',  ( 24.71252020198295085, 8.768263569673496960, -0.7333271064221494884 ) ) ;
#10586 = AXIS2_PLACEMENT_3D ( 'NONE', #3645, #7064, #2079 ) ;
#10588 = CARTESIAN_POINT ( 'NONE',  ( 14.07100346269973201, -6.903878524309663867, -15.26435492765976321 ) ) ;
#10587 = LINE ( 'NONE', #5166, #4209 ) ;
#10589 = ORIENTED_EDGE ( 'NONE', *, *, #19696, .T. ) ;
#10590 = ORIENTED_EDGE ( 'NONE', *, *, #16837, .T. ) ;
#10591 = CARTESIAN_POINT ( 'NONE',  ( 13.83162162704461373, 20.92405235932746166, 3.372942155665883401 ) ) ;
#10593 = CARTESIAN_POINT ( 'NONE',  ( -17.16618386210371483, -6.903720000000000745, 58.07004290071009223 ) ) ;
#10592 = CARTESIAN_POINT ( 'NONE',  ( 5.012423084987765343, 21.41828792979770313, 1.984503165450502538 ) ) ;
#10594 = ORIENTED_EDGE ( 'NONE', *, *, #20990, .T. ) ;
#10596 = CARTESIAN_POINT ( 'NONE',  ( 20.46393712135811072, -0.2355988221118890391, -15.20378812335061092 ) ) ;
#10595 = CARTESIAN_POINT ( 'NONE',  ( 5.430225438562612972, 12.90007726256580689, 7.561889016175808109 ) ) ;
#10597 = EDGE_LOOP ( 'NONE', ( #18246, #13716, #19560, #17375, #5009, #19640 ) ) ;
#10598 = VECTOR ( 'NONE', #14447, 1000.000000000000114 ) ;
#10599 = ORIENTED_EDGE ( 'NONE', *, *, #11055, .F. ) ;
#10600 = EDGE_CURVE ( 'NONE', #14925, #18990, #20559, .T. ) ;
#10601 = CARTESIAN_POINT ( 'NONE',  ( 7.842133636678705777, 12.16369228495859645, 0.2595828833526279689 ) ) ;
#10602 = ORIENTED_EDGE ( 'NONE', *, *, #2511, .T. ) ;
#10603 = VECTOR ( 'NONE', #11863, 1000.000000000000000 ) ;
#10604 = VECTOR ( 'NONE', #15444, 1000.000000000000000 ) ;
#10605 = EDGE_CURVE ( 'NONE', #20984, #11600, #13974, .T. ) ;
#10606 = EDGE_CURVE ( 'NONE', #21599, #7998, #9288, .T. ) ;
#10607 = LINE ( 'NONE', #10492, #16676 ) ;
#10608 = CARTESIAN_POINT ( 'NONE',  ( 38.32938179974708959, -7.102284129468043439, -4.721977392770211779 ) ) ;
#10609 = LINE ( 'NONE', #19324, #13252 ) ;
#10610 = CARTESIAN_POINT ( 'NONE',  ( 1.814948966250774065, 21.19546389864396119, 4.850479613994575168 ) ) ;
#10611 = CARTESIAN_POINT ( 'NONE',  ( 61.60152099976809126, 37.11476346399999926, -12.48877542598203405 ) ) ;
#10612 = CIRCLE ( 'NONE', #1075, 1.190625000000000711 ) ;
#10613 = ORIENTED_EDGE ( 'NONE', *, *, #9226, .T. ) ;
#10614 = CARTESIAN_POINT ( 'NONE',  ( 48.78323016782857735, -1.983739999999999837, -25.79158832643865651 ) ) ;
#10615 = CARTESIAN_POINT ( 'NONE',  ( 13.05845502804394798, 21.54598149573345367, 1.959600843863859243 ) ) ;
#10616 = DIRECTION ( 'NONE',  ( 0.000000000000000000, -1.000000000000000000, 0.000000000000000000 ) ) ;
#10617 = ORIENTED_EDGE ( 'NONE', *, *, #8649, .T. ) ;
#10618 = ORIENTED_EDGE ( 'NONE', *, *, #12304, .F. ) ;
#10619 = CARTESIAN_POINT ( 'NONE',  ( 13.26602609393551369, 22.11716190621255862, 2.502407145256026588 ) ) ;
#10620 = AXIS2_PLACEMENT_3D ( 'NONE', #10682, #6914, #13677 ) ;
#10621 = CARTESIAN_POINT ( 'NONE',  ( -5.863861779363051419, 34.12394749999999988, -34.80955303575778714 ) ) ;
#10622 = CARTESIAN_POINT ( 'NONE',  ( 11.53730135053356776, 11.04591141993689263, -1.177169684089045765 ) ) ;
#10623 = VERTEX_POINT ( 'NONE', #20671 ) ;
#10624 = ORIENTED_EDGE ( 'NONE', *, *, #16023, .T. ) ;
#10625 = CARTESIAN_POINT ( 'NONE',  ( 49.81956284419040060, 0.000000000000000000, 11.98436472153758103 ) ) ;
#10626 = CARTESIAN_POINT ( 'NONE',  ( 7.496787083349086167, 18.49057725868834723, -2.494173209474321862 ) ) ;
#10627 = CARTESIAN_POINT ( 'NONE',  ( 3.425778229864998359, 16.48230391985759979, 8.522309372965072072 ) ) ;
#10628 = CARTESIAN_POINT ( 'NONE',  ( 1.890011456818353031, 34.09881183566065488, -22.67530205718465908 ) ) ;
#10629 = EDGE_CURVE ( 'NONE', #218, #16113, #19244, .T. ) ;
#10630 = CARTESIAN_POINT ( 'NONE',  ( 5.732870978699193820, 17.39963396565737952, -1.291407831173700282 ) ) ;
#10631 = EDGE_CURVE ( 'NONE', #9499, #18470, #2332, .T. ) ;
#10632 = ADVANCED_FACE ( 'NONE', ( #12185 ), #9171, .F. ) ;
#10633 = VECTOR ( 'NONE', #13461, 1000.000000000000000 ) ;
#10634 = FACE_OUTER_BOUND ( 'NONE', #21786, .T. ) ;
#10635 = CARTESIAN_POINT ( 'NONE',  ( 5.777562495344723992, 17.39297272447799614, -2.183326841469702906 ) ) ;
#10636 = CARTESIAN_POINT ( 'NONE',  ( 4.689920459349973036, 11.91097906394028172, 4.285078460903785746 ) ) ;
#10637 = AXIS2_PLACEMENT_3D ( 'NONE', #2462, #14415, #17723 ) ;
#10638 = CARTESIAN_POINT ( 'NONE',  ( 13.45333066700820979, 21.38713583945818542, 1.818036823379868938 ) ) ;
#10639 = CARTESIAN_POINT ( 'NONE',  ( 0.6492888148354383215, 20.32382785537196312, 1.812354305104474150 ) ) ;
#10640 = CARTESIAN_POINT ( 'NONE',  ( 0.2710380737689748187, 20.85778803320007313, 6.370138859128364750 ) ) ;
#10641 = DIRECTION ( 'NONE',  ( -0.2490110332224855227, 0.000000000000000000, 0.9685006480810791629 ) ) ;
#10642 = CARTESIAN_POINT ( 'NONE',  ( 7.264882008937790125, 16.58796963715414208, 7.727752318332806958 ) ) ;
#10643 = LINE ( 'NONE', #5873, #5298 ) ;
#10644 = FACE_OUTER_BOUND ( 'NONE', #16503, .T. ) ;
#10645 = CARTESIAN_POINT ( 'NONE',  ( 20.95242871594548362, -3.348541484849226535, -13.87224525169349043 ) ) ;
#10646 = DIRECTION ( 'NONE',  ( -0.9579671649362034858, 0.000000000000000000, 0.2868778675745011220 ) ) ;
#10647 = VECTOR ( 'NONE', #11221, 1000.000000000000114 ) ;
#10648 = DIRECTION ( 'NONE',  ( 1.000000000000000000, 0.000000000000000000, 0.000000000000000000 ) ) ;
#10649 = CARTESIAN_POINT ( 'NONE',  ( 11.27183014273422401, 12.74897102812991179, 6.369117077617454825 ) ) ;
#10650 = EDGE_LOOP ( 'NONE', ( #13491, #2936, #8680, #11352 ) ) ;
#10651 = DIRECTION ( 'NONE',  ( 0.9685006480810792739, 0.000000000000000000, 0.2490110332224853007 ) ) ;
#10652 = AXIS2_PLACEMENT_3D ( 'NONE', #20544, #19228, #10398 ) ;
#10653 = CARTESIAN_POINT ( 'NONE',  ( 11.79451413562702911, 11.46334091281098111, -0.1568912284302553251 ) ) ;
#10654 = DIRECTION ( 'NONE',  ( 0.000000000000000000, 1.000000000000000000, 0.000000000000000000 ) ) ;
#10655 = CARTESIAN_POINT ( 'NONE',  ( -0.07820122749697261400, 15.70581984897159700, 0.7984465916195991886 ) ) ;
#10656 = EDGE_LOOP ( 'NONE', ( #15656, #17616 ) ) ;
#10657 = PRODUCT_CONTEXT ( 'NONE', #12720, 'mechanical' ) ;
#10658 = DIRECTION ( 'NONE',  ( 1.000000000000000000, 0.000000000000000000, 0.000000000000000000 ) ) ;
#10659 = CARTESIAN_POINT ( 'NONE',  ( 4.932957014358739123, 20.42853515389766272, 1.908948791967717273 ) ) ;
#10660 = EDGE_CURVE ( 'NONE', #9895, #11597, #14078, .T. ) ;
#10661 = LINE ( 'NONE', #373, #867 ) ;
#10662 = VECTOR ( 'NONE', #17502, 1000.000000000000000 ) ;
#10663 = TOROIDAL_SURFACE ( 'NONE', #1808, 3.174999999999999822, 1.190625000000000044 ) ;
#10664 = CARTESIAN_POINT ( 'NONE',  ( 21.56733905798141393, -3.402205227929565812, -14.90816191201569474 ) ) ;
#10665 = EDGE_LOOP ( 'NONE', ( #20095, #20836, #2811, #11978, #3389, #17198, #20308, #14285, #17873, #8269, #20388, #10617 ) ) ;
#10666 = CARTESIAN_POINT ( 'NONE',  ( 12.97628609860860394, 18.46234326053249220, 6.039901028563929408 ) ) ;
#10667 = CARTESIAN_POINT ( 'NONE',  ( 5.709010112337018938, 17.24330370537085955, -1.425333744364522648 ) ) ;
#10668 = CYLINDRICAL_SURFACE ( 'NONE', #14951, 1.587499999999999911 ) ;
#10669 = AXIS2_PLACEMENT_3D ( 'NONE', #5263, #19086, #6935 ) ;
#10670 = CIRCLE ( 'NONE', #3252, 30.16250000000000497 ) ;
#10671 = DIRECTION ( 'NONE',  ( 0.000000000000000000, -1.000000000000000000, 0.000000000000000000 ) ) ;
#10672 = CARTESIAN_POINT ( 'NONE',  ( 15.75244874201758094, 1.099573029051923667, -15.53104562322756088 ) ) ;
#10673 = DIRECTION ( 'NONE',  ( -0.9790635044817342925, 0.000000000000000000, 0.2035550397114870846 ) ) ;
#10674 = ORIENTED_EDGE ( 'NONE', *, *, #17617, .F. ) ;
#10675 = CARTESIAN_POINT ( 'NONE',  ( 11.20683540457644334, 15.87299087032793743, 6.798486701180226355 ) ) ;
#10676 = CARTESIAN_POINT ( 'NONE',  ( 12.65066698874035112, 20.52417811251926238, 5.611220316870539904 ) ) ;
#10677 = CARTESIAN_POINT ( 'NONE',  ( 10.10534066920194185, -95.96551800000000298, -14.00784516691476966 ) ) ;
#10678 = AXIS2_PLACEMENT_3D ( 'NONE', #6172, #969, #19868 ) ;
#10679 = ORIENTED_EDGE ( 'NONE', *, *, #12848, .T. ) ;
#10680 = CIRCLE ( 'NONE', #18377, 3.175000000000000711 ) ;
#10681 = CARTESIAN_POINT ( 'NONE',  ( 10.51247066191329083, 11.49109188741821264, 3.088008306483761789 ) ) ;
#10682 = CARTESIAN_POINT ( 'NONE',  ( 9.133321157616299146, 13.08957250000000094, -4.290529607290007874 ) ) ;
#10683 = DIRECTION ( 'NONE',  ( -0.9488823340533351081, -0.2002559181062071036, -0.2439669719140995230 ) ) ;
#10685 = DIRECTION ( 'NONE',  ( -0.9790635044817341814, 0.000000000000000000, 0.2035550397114869736 ) ) ;
#10684 = CARTESIAN_POINT ( 'NONE',  ( 1.717996366984696488, 12.18301083390420203, 2.082593322157058946 ) ) ;
#10686 = ORIENTED_EDGE ( 'NONE', *, *, #12438, .T. ) ;
#10687 = EDGE_CURVE ( 'NONE', #12517, #11596, #14076, .T. ) ;
#10688 = FACE_OUTER_BOUND ( 'NONE', #4156, .T. ) ;
#10689 = VERTEX_POINT ( 'NONE', #5645 ) ;
#10690 = CIRCLE ( 'NONE', #8213, 9.524999999999996803 ) ;
#10691 = CARTESIAN_POINT ( 'NONE',  ( 19.58283533066354565, 0.2704557082564330583, -14.92202265744526990 ) ) ;
#10692 = CARTESIAN_POINT ( 'NONE',  ( 20.34020935552985065, -3.329038851323427917, -15.20636776770394683 ) ) ;
#10693 = VERTEX_POINT ( 'NONE', #785 ) ;
#10694 = DIRECTION ( 'NONE',  ( 0.000000000000000000, -1.000000000000000000, -0.000000000000000000 ) ) ;
#10695 = AXIS2_PLACEMENT_3D ( 'NONE', #17323, #19080, #7485 ) ;
#10696 = EDGE_CURVE ( 'NONE', #19764, #9048, #17943, .T. ) ;
#10697 = DIRECTION ( 'NONE',  ( 0.000000000000000000, 1.000000000000000000, 0.000000000000000000 ) ) ;
#10698 = LINE ( 'NONE', #18970, #5186 ) ;
#10699 = CIRCLE ( 'NONE', #16357, 3.970019999999998550 ) ;
#10700 = ORIENTED_EDGE ( 'NONE', *, *, #20682, .T. ) ;
#10701 = CARTESIAN_POINT ( 'NONE',  ( 60.38511073144201191, -1.983739999999999837, -22.26373525985038526 ) ) ;
#10702 = LINE ( 'NONE', #17447, #13498 ) ;
#10703 = DIRECTION ( 'NONE',  ( 0.000000000000000000, -1.000000000000000000, 0.000000000000000000 ) ) ;
#10705 = LINE ( 'NONE', #12810, #2396 ) ;
#10704 = FACE_BOUND ( 'NONE', #2470, .T. ) ;
#10706 = ORIENTED_EDGE ( 'NONE', *, *, #3973, .T. ) ;
#10707 = ORIENTED_EDGE ( 'NONE', *, *, #20673, .F. ) ;
#10709 = LINE ( 'NONE', #15482, #12439 ) ;
#10708 = CARTESIAN_POINT ( 'NONE',  ( 1.686968993106074510, 16.44735884859098718, -0.8025552312217851814 ) ) ;
#10710 = EDGE_LOOP ( 'NONE', ( #11161, #11707, #13605, #18213, #21538, #15054 ) ) ;
#10712 = CARTESIAN_POINT ( 'NONE',  ( 17.20754637584470714, -7.943092760107163919, -15.14184226529886246 ) ) ;
#10711 = CARTESIAN_POINT ( 'NONE',  ( 4.997041246908954015, 11.45262702614296302, 5.581120543604684237 ) ) ;
#10713 = AXIS2_PLACEMENT_3D ( 'NONE', #9380, #1203, #2865 ) ;
#10714 = ORIENTED_EDGE ( 'NONE', *, *, #18516, .T. ) ;
#10715 = EDGE_CURVE ( 'NONE', #16893, #5161, #20043, .T. ) ;
#10716 = VERTEX_POINT ( 'NONE', #2101 ) ;
#10717 = EDGE_CURVE ( 'NONE', #14160, #5388, #21220, .T. ) ;
#10718 = AXIS2_PLACEMENT_3D ( 'NONE', #12735, #9291, #19459 ) ;
#10719 = ORIENTED_EDGE ( 'NONE', *, *, #641, .F. ) ;
#10720 = CARTESIAN_POINT ( 'NONE',  ( 3.139362194088404667, 12.70870594642470230, 6.498606875045355835 ) ) ;
#10721 = DIRECTION ( 'NONE',  ( 0.000000000000000000, 1.000000000000000000, 0.000000000000000000 ) ) ;
#10722 = VECTOR ( 'NONE', #16514, 1000.000000000000000 ) ;
#10723 = CARTESIAN_POINT ( 'NONE',  ( -3.246390552019219999, 12.30439499999999953, 3.217431771123079987 ) ) ;
#10724 = CARTESIAN_POINT ( 'NONE',  ( 54.72004008979249789, -6.356984999999999886, -15.77242863567076014 ) ) ;
#10725 = CARTESIAN_POINT ( 'NONE',  ( 3.564885292549716311, 16.92788500666243223, 9.175419982453322021 ) ) ;
#10726 = ORIENTED_EDGE ( 'NONE', *, *, #20965, .T. ) ;
#10727 = CARTESIAN_POINT ( 'NONE',  ( 4.318272399054353450, 20.61711312421807918, 4.992195515787562599 ) ) ;
#10728 = CARTESIAN_POINT ( 'NONE',  ( 11.68644878885729277, -4.515843508674393547, -16.26277472245715927 ) ) ;
#10729 = CARTESIAN_POINT ( 'NONE',  ( 13.39756118469465029, 22.16307784260286340, 1.948616576935187750 ) ) ;
#10730 = DIRECTION ( 'NONE',  ( -0.9964481331860213231, 0.000000000000000000, 0.08420877549337293932 ) ) ;
#10731 = ADVANCED_FACE ( 'NONE', ( #9722 ), #16486, .F. ) ;
#10732 = FACE_OUTER_BOUND ( 'NONE', #6304, .T. ) ;
#10733 = ORIENTED_EDGE ( 'NONE', *, *, #6830, .T. ) ;
#10734 = ORIENTED_EDGE ( 'NONE', *, *, #498, .T. ) ;
#10735 = CARTESIAN_POINT ( 'NONE',  ( 8.812473556068928460, 13.52835235745250131, -2.451387110162866367 ) ) ;
#10736 = DIRECTION ( 'NONE',  ( 0.2868778675745011220, 0.000000000000000000, 0.9579671649362034858 ) ) ;
#10737 = CARTESIAN_POINT ( 'NONE',  ( 13.02604791969851661, 11.75039870752145177, 5.077274524504193032 ) ) ;
#10738 = ORIENTED_EDGE ( 'NONE', *, *, #20717, .T. ) ;
#10739 = ORIENTED_EDGE ( 'NONE', *, *, #17168, .F. ) ;
#10740 = DIRECTION ( 'NONE',  ( 0.9685006480810792739, 0.000000000000000000, 0.2490110332224846346 ) ) ;
#10741 = CARTESIAN_POINT ( 'NONE',  ( 7.877529856632134120, 20.02306472266900172, -1.583040783571615151 ) ) ;
#10742 = CARTESIAN_POINT ( 'NONE',  ( 54.61912012054379062, -6.356984999999999886, -13.79062155615056362 ) ) ;
#10743 = CARTESIAN_POINT ( 'NONE',  ( 1.998220421679061776, 34.04486736277070236, -22.64748046904500356 ) ) ;
#10744 = EDGE_CURVE ( 'NONE', #13013, #7142, #21112, .T. ) ;
#10745 = CARTESIAN_POINT ( 'NONE',  ( 5.592841715996570429, 15.66352912673956865, -1.341337588800156411 ) ) ;
#10746 = AXIS2_PLACEMENT_3D ( 'NONE', #12047, #11834, #103 ) ;
#10747 = CARTESIAN_POINT ( 'NONE',  ( 1.532169971477637782, 5.548947500000001476, -20.71839214105750315 ) ) ;
#10748 = CARTESIAN_POINT ( 'NONE',  ( 9.452961308647887861, 13.36844392990906272, -2.929793466363328491 ) ) ;
#10749 = APPLICATION_CONTEXT ( 'automotive_design' ) ;
#10750 = VECTOR ( 'NONE', #7617, 1000.000000000000114 ) ;
#10751 = CARTESIAN_POINT ( 'NONE',  ( -3.845402119898529758, 28.56769750000000130, -31.39393985263922460 ) ) ;
#10752 = CARTESIAN_POINT ( 'NONE',  ( 1.700980557147387717, 15.58904521221044170, 9.664144641518724654 ) ) ;
#10753 = CARTESIAN_POINT ( 'NONE',  ( 0.2748101640027249548, 20.85481667080186341, 6.380173850233394006 ) ) ;
#10754 = CARTESIAN_POINT ( 'NONE',  ( 0.7950072837654299507, 19.66973114709098169, 2.266613654961380675 ) ) ;
#10755 = DIRECTION ( 'NONE',  ( 0.000000000000000000, 0.000000000000000000, 1.000000000000000000 ) ) ;
#10756 = CARTESIAN_POINT ( 'NONE',  ( 9.058884679750676128, 128.5105379999999968, -16.32319115207028659 ) ) ;
#10757 = CARTESIAN_POINT ( 'NONE',  ( 19.74951347795774481, 0.4024288987411958618, -14.32971591649493170 ) ) ;
#10758 = EDGE_CURVE ( 'NONE', #9392, #13313, #14503, .T. ) ;
#10759 = CIRCLE ( 'NONE', #21687, 9.525000000000002132 ) ;
#10760 = EDGE_CURVE ( 'NONE', #20009, #18286, #19572, .T. ) ;
#10761 = DIRECTION ( 'NONE',  ( 0.7421532822901579785, 0.000000000000000000, -0.6702301885068630005 ) ) ;
#10762 = EDGE_CURVE ( 'NONE', #15942, #3338, #13794, .T. ) ;
#10763 = CARTESIAN_POINT ( 'NONE',  ( 29.64606458365116737, 1.975802500000001904, -15.53894806404596096 ) ) ;
#10764 = CARTESIAN_POINT ( 'NONE',  ( 9.798027642257455483, 10.93122598874641049, 0.05745448286648872915 ) ) ;
#10765 = ORIENTED_EDGE ( 'NONE', *, *, #16040, .T. ) ;
#10766 = DIRECTION ( 'NONE',  ( 0.000000000000000000, -1.000000000000000000, -0.000000000000000000 ) ) ;
#10767 = CARTESIAN_POINT ( 'NONE',  ( 11.14545677980454208, 15.43789734212750808, -3.509883341676725443 ) ) ;
#10768 = CARTESIAN_POINT ( 'NONE',  ( 5.541718124298840031, 12.84840258351819209, -0.8988864716115243514 ) ) ;
#10769 = DIRECTION ( 'NONE',  ( 0.000000000000000000, -1.000000000000000000, 0.000000000000000000 ) ) ;
#10770 = CARTESIAN_POINT ( 'NONE',  ( 3.307247859361858389, 16.48205525895870593, 8.552608352040381945 ) ) ;
#10771 = VECTOR ( 'NONE', #19621, 1000.000000000000227 ) ;
#10772 = VERTEX_POINT ( 'NONE', #11903 ) ;
#10773 = DIRECTION ( 'NONE',  ( -0.000000000000000000, 1.000000000000000000, 0.000000000000000000 ) ) ;
#10774 = CIRCLE ( 'NONE', #16080, 0.7950200000000003930 ) ;
#10775 = VERTEX_POINT ( 'NONE', #8785 ) ;
#10776 = CARTESIAN_POINT ( 'NONE',  ( 8.115118250563648772, 19.55588805595618140, -1.118609513322449622 ) ) ;
#10777 = CARTESIAN_POINT ( 'NONE',  ( 13.54495441322193372, 21.41280428856536489, 2.252596376362126396 ) ) ;
#10778 = CARTESIAN_POINT ( 'NONE',  ( 46.03750000000000142, 42.06303499999999929, -10.31874999999999964 ) ) ;
#10779 = ADVANCED_FACE ( 'NONE', ( #17200 ), #15456, .F. ) ;
#10780 = CARTESIAN_POINT ( 'NONE',  ( 19.29498493895778211, -0.9933881662693676562, -14.41052274056791305 ) ) ;
#10781 = UNCERTAINTY_MEASURE_WITH_UNIT (LENGTH_MEASURE( 1.000000000000000082E-05 ), #3721, 'distance_accuracy_value', 'NONE');
#10782 = ADVANCED_FACE ( 'NONE', ( #10353 ), #17435, .T. ) ;
#10783 = DIRECTION ( 'NONE',  ( -0.3928209820863007296, 0.000000000000000000, 0.9196149607486571176 ) ) ;
#10784 = VERTEX_POINT ( 'NONE', #1836 ) ;
#10785 = CARTESIAN_POINT ( 'NONE',  ( 11.20894518263242112, 14.54054042788871648, 6.496243861428408373 ) ) ;
#10786 = CARTESIAN_POINT ( 'NONE',  ( 11.43530489704916420, 13.68296282620402238, 7.076276842477176032 ) ) ;
#10787 = AXIS2_PLACEMENT_3D ( 'NONE', #6060, #6274, #2861 ) ;
#10788 = ORIENTED_EDGE ( 'NONE', *, *, #3563, .T. ) ;
#10789 = CARTESIAN_POINT ( 'NONE',  ( 9.293274126941451385, 15.02556043177791878, -2.679682145362060730 ) ) ;
#10790 = FACE_OUTER_BOUND ( 'NONE', #19770, .T. ) ;
#10791 = DIRECTION ( 'NONE',  ( 0.000000000000000000, 1.000000000000000000, -0.000000000000000000 ) ) ;
#10793 = CARTESIAN_POINT ( 'NONE',  ( 21.43124999999999858, 16.27314499999999953, 8.731249999999999289 ) ) ;
#10792 = CARTESIAN_POINT ( 'NONE',  ( 3.588507411891436405, 18.91035477026892409, -0.3510181181459797739 ) ) ;
#10794 = ORIENTED_EDGE ( 'NONE', *, *, #20187, .T. ) ;
#10795 = CARTESIAN_POINT ( 'NONE',  ( 7.115159381822890872, 11.75569977924905274, 5.947017350195187291 ) ) ;
#10796 = DIRECTION ( 'NONE',  ( 0.2490110332224850509, 0.000000000000000000, -0.9685006480810792739 ) ) ;
#10797 = CARTESIAN_POINT ( 'NONE',  ( 39.70735255319233659, -6.957959099329872998, -3.201272008584183482 ) ) ;
#10798 = VERTEX_POINT ( 'NONE', #8575 ) ;
#10799 = CARTESIAN_POINT ( 'NONE',  ( 19.34116629174159030, 0.4109076020908116189, -15.03439639987123755 ) ) ;
#10800 = CARTESIAN_POINT ( 'NONE',  ( 17.18860471232197540, -7.336512682313781397, -15.77586843043927267 ) ) ;
#10801 = EDGE_LOOP ( 'NONE', ( #2391, #20208, #18629, #15703 ) ) ;
#10802 = LINE ( 'NONE', #21068, #8554 ) ;
#10803 = VECTOR ( 'NONE', #11969, 1000.000000000000000 ) ;
#10804 = CARTESIAN_POINT ( 'NONE',  ( 11.58758032897313761, 10.98269117049956201, -1.359133207363109941 ) ) ;
#10805 = CARTESIAN_POINT ( 'NONE',  ( -18.18961309330695997, -3.266559801243759331, -25.80119252674831998 ) ) ;
#10806 = ADVANCED_FACE ( 'NONE', ( #17096 ), #18959, .T. ) ;
#10807 = CARTESIAN_POINT ( 'NONE',  ( 55.56250000000000000, 32.54502000000000095, -10.31874999999999964 ) ) ;
#10808 = ORIENTED_EDGE ( 'NONE', *, *, #13339, .T. ) ;
#10809 = DIRECTION ( 'NONE',  ( -0.6744690509234934073, 0.7360996206939023345, 0.05699866455150641442 ) ) ;
#10811 = CARTESIAN_POINT ( 'NONE',  ( 65.90927232300019512, 1.984375000000000000, -13.30734117861468135 ) ) ;
#10810 = DIRECTION ( 'NONE',  ( 0.000000000000000000, -1.000000000000000000, 0.000000000000000000 ) ) ;
#10812 = VERTEX_POINT ( 'NONE', #12342 ) ;
#10813 = VERTEX_POINT ( 'NONE', #15351 ) ;
#10815 = CARTESIAN_POINT ( 'NONE',  ( 21.03437500000000071, 32.54502000000000095, 5.159374999999999822 ) ) ;
#10814 = CARTESIAN_POINT ( 'NONE',  ( 1.657404189593110644, 14.62646646242487769, -0.5067450003820986870 ) ) ;
#10816 = EDGE_LOOP ( 'NONE', ( #18524, #16629, #18554, #20193, #2765, #7860 ) ) ;
#10817 = CARTESIAN_POINT ( 'NONE',  ( 5.489998326203298973, 17.16039541831715454, 8.734701079443423666 ) ) ;
#10818 = ORIENTED_EDGE ( 'NONE', *, *, #16672, .T. ) ;
#10819 = ORIENTED_EDGE ( 'NONE', *, *, #20484, .F. ) ;
#10820 = ORIENTED_EDGE ( 'NONE', *, *, #14699, .T. ) ;
#10821 = CARTESIAN_POINT ( 'NONE',  ( 3.067686375243920072, 12.50340986505852747, 6.152773509231688642 ) ) ;
#10822 = CARTESIAN_POINT ( 'NONE',  ( -1.724236557342190057, 0.000000000000000000, 8.786659759980359752 ) ) ;
#10823 = DIRECTION ( 'NONE',  ( 0.000000000000000000, 1.000000000000000000, 0.000000000000000000 ) ) ;
#10824 = CARTESIAN_POINT ( 'NONE',  ( 17.10576967688479399, -14.84248999999999974, -11.38708898545455561 ) ) ;
#10825 = CARTESIAN_POINT ( 'NONE',  ( 1.765172365516369579, 21.20083304101597221, 4.716146812010884481 ) ) ;
#10826 = EDGE_CURVE ( 'NONE', #11404, #21357, #13683, .T. ) ;
#10827 = ORIENTED_EDGE ( 'NONE', *, *, #13387, .F. ) ;
#10828 = CARTESIAN_POINT ( 'NONE',  ( 3.751596593617982478, 20.73071249212684108, 3.494438650925056233 ) ) ;
#10829 = PLANE ( 'NONE',  #7132 ) ;
#10830 = DIRECTION ( 'NONE',  ( 0.000000000000000000, -1.000000000000000000, 0.000000000000000000 ) ) ;
#10831 = CARTESIAN_POINT ( 'NONE',  ( 0.02083138522551555155, 20.24316500000000119, 7.210477125664100484 ) ) ;
#10832 = DIRECTION ( 'NONE',  ( 0.000000000000000000, 1.000000000000000000, 0.000000000000000000 ) ) ;
#10833 = VERTEX_POINT ( 'NONE', #20384 ) ;
#10834 = ORIENTED_EDGE ( 'NONE', *, *, #17833, .F. ) ;
#10835 = CARTESIAN_POINT ( 'NONE',  ( 5.656518577322932728, 11.49185006667808118, 1.607793118288020962 ) ) ;
#10836 = CIRCLE ( 'NONE', #3784, 1.190625000000000711 ) ;
#10838 = CARTESIAN_POINT ( 'NONE',  ( 32.10373694497760511, -6.356984999999999886, -3.785462747693984831 ) ) ;
#10837 = PLANE ( 'NONE',  #20700 ) ;
#10839 = CARTESIAN_POINT ( 'NONE',  ( 13.23440871943589237, 12.81420739021140598, 6.047183941140541030 ) ) ;
#10840 = ORIENTED_EDGE ( 'NONE', *, *, #311, .F. ) ;
#10841 = ORIENTED_EDGE ( 'NONE', *, *, #11667, .F. ) ;
#10842 = LINE ( 'NONE', #14293, #2501 ) ;
#10843 = CARTESIAN_POINT ( 'NONE',  ( 7.308308794374226203, 17.13478947702074251, -2.844519879704227705 ) ) ;
#10844 = CARTESIAN_POINT ( 'NONE',  ( 30.33489826846160398, 0.000000000000000000, -2.417033907079745525 ) ) ;
#10845 = DIRECTION ( 'NONE',  ( -0.9790635044817341814, 0.000000000000000000, 0.2035550397114869736 ) ) ;
#10846 = CARTESIAN_POINT ( 'NONE',  ( 5.656977408468667257, 13.81142017241615605, -0.6512533121070646080 ) ) ;
#10847 = CYLINDRICAL_SURFACE ( 'NONE', #5775, 0.5079999999999963434 ) ;
#10848 = EDGE_CURVE ( 'NONE', #6259, #14245, #3832, .T. ) ;
#10849 = AXIS2_PLACEMENT_3D ( 'NONE', #14144, #17659, #12806 ) ;
#10850 = CARTESIAN_POINT ( 'NONE',  ( 13.72939367483574280, 14.76516699303951619, 6.561508169267058932 ) ) ;
#10851 = CARTESIAN_POINT ( 'NONE',  ( 3.524129415282716060, 13.11356558266398231, 8.223647746374714629 ) ) ;
#10852 = CARTESIAN_POINT ( 'NONE',  ( 24.60624999999999929, 16.27314499999999953, 8.731249999999999289 ) ) ;
#10853 = EDGE_CURVE ( 'NONE', #1480, #8937, #15236, .T. ) ;
#10854 = ADVANCED_FACE ( 'NONE', ( #5250 ), #6816, .F. ) ;
#10855 = ADVANCED_FACE ( 'NONE', ( #3498 ), #8682, .F. ) ;
#10856 = PLANE ( 'NONE',  #2585 ) ;
#10857 = CARTESIAN_POINT ( 'NONE',  ( 2.356114889612781482, 20.09535866699502193, 6.295991311034685012 ) ) ;
#10858 = DIRECTION ( 'NONE',  ( 0.9959941601142464629, 0.000000000000000000, 0.08941830359784661009 ) ) ;
#10859 = DIRECTION ( 'NONE',  ( 0.000000000000000000, -1.000000000000000000, 0.000000000000000000 ) ) ;
#10860 = CARTESIAN_POINT ( 'NONE',  ( 20.05460976202589407, -0.006649262762246921366, -14.23230800686313735 ) ) ;
#10861 = ORIENTED_EDGE ( 'NONE', *, *, #19953, .F. ) ;
#10862 = CARTESIAN_POINT ( 'NONE',  ( -16.88621914012359326, 35.81157980123359863, -10.37804376527844141 ) ) ;
#10863 = CARTESIAN_POINT ( 'NONE',  ( 26.59062499828754866, 30.56080374999745075, 10.71562494918373964 ) ) ;
#10864 = CARTESIAN_POINT ( 'NONE',  ( 11.43263507844261007, 14.55322455989931107, 7.303294973855595451 ) ) ;
#10865 = ORIENTED_EDGE ( 'NONE', *, *, #8323, .T. ) ;
#10866 = CARTESIAN_POINT ( 'NONE',  ( 9.058884679750676128, 34.52875999999999834, -16.32319115207028659 ) ) ;
#10867 = CARTESIAN_POINT ( 'NONE',  ( 11.42389331219130177, 18.34427701479485506, -3.218461924845117395 ) ) ;
#10868 = CARTESIAN_POINT ( 'NONE',  ( 5.376858612653267144, 15.95884149645304007, -2.144506965101294682 ) ) ;
#10869 = LINE ( 'NONE', #7766, #2796 ) ;
#10870 = ORIENTED_EDGE ( 'NONE', *, *, #896, .T. ) ;
#10871 = CARTESIAN_POINT ( 'NONE',  ( 5.623588726797621895, 20.73702223218877094, 3.727985457070243314 ) ) ;
#10872 = CARTESIAN_POINT ( 'NONE',  ( 38.94885947252247860, -7.547248457916676756, -3.956611957470116625 ) ) ;
#10873 = ADVANCED_FACE ( 'NONE', ( #2161 ), #8905, .F. ) ;
#10874 = CARTESIAN_POINT ( 'NONE',  ( 21.03649535373696722, -1.171894805719116084, -15.12491633086513687 ) ) ;
#10875 = ORIENTED_EDGE ( 'NONE', *, *, #5220, .T. ) ;
#10876 = CARTESIAN_POINT ( 'NONE',  ( 5.654395174991643458, 15.56639808041640372, -1.444955789142327029 ) ) ;
#10877 = CARTESIAN_POINT ( 'NONE',  ( 11.23643128109388201, 14.04470801367943267, 6.379844766020851488 ) ) ;
#10878 = DIRECTION ( 'NONE',  ( -0.7421532822901572013, 0.000000000000000000, 0.6702301885068637777 ) ) ;
#10879 = ADVANCED_FACE ( 'NONE', ( #10688 ), #619, .T. ) ;
#10880 = DIRECTION ( 'NONE',  ( -0.9784543669157944601, 0.000000000000000000, -0.2064631973582987667 ) ) ;
#10881 = CARTESIAN_POINT ( 'NONE',  ( 4.065274381575306961, 21.20935756750483137, 5.231433629464312673 ) ) ;
#10882 = CARTESIAN_POINT ( 'NONE',  ( 59.80894853325292360, -6.356984999999999886, -16.70545285374888778 ) ) ;
#10883 = SHAPE_REPRESENTATION ( 'Locking Pawl Compression Spring', ( #2234 ), #652 ) ;
#10884 = ORIENTED_EDGE ( 'NONE', *, *, #1308, .T. ) ;
#10885 =( GEOMETRIC_REPRESENTATION_CONTEXT ( 3 ) GLOBAL_UNCERTAINTY_ASSIGNED_CONTEXT ( ( #4144 ) ) GLOBAL_UNIT_ASSIGNED_CONTEXT ( ( #9340, #20254, #10207 ) ) REPRESENTATION_CONTEXT ( 'NONE', 'WORKASPACE' ) );
#10886 = CARTESIAN_POINT ( 'NONE',  ( 9.280893739159276734, 12.85627548497952155, 6.982956407158277479 ) ) ;
#10887 = CARTESIAN_POINT ( 'NONE',  ( 52.29466199406144966, 39.42598491866655763, -17.50029076404656792 ) ) ;
#10888 = VERTEX_POINT ( 'NONE', #10896 ) ;
#10889 = CARTESIAN_POINT ( 'NONE',  ( 9.808641443463722354, 11.80443358965426270, 0.01604935767821101880 ) ) ;
#10890 = LINE ( 'NONE', #2604, #15901 ) ;
#10891 = CARTESIAN_POINT ( 'NONE',  ( 1.181662039134980802, 18.03831543248292846, 8.489857044810902309 ) ) ;
#10893 = CARTESIAN_POINT ( 'NONE',  ( -19.99570496368815142, 42.13594019876639862, -10.11526441440630286 ) ) ;
#10892 = CARTESIAN_POINT ( 'NONE',  ( 4.597652426504708068, 21.03084409073214189, 2.229734299069735748 ) ) ;
#10894 = ORIENTED_EDGE ( 'NONE', *, *, #20692, .T. ) ;
#10895 = DIRECTION ( 'NONE',  ( 1.000000000000000000, 0.000000000000000000, 0.000000000000000000 ) ) ;
#10896 = CARTESIAN_POINT ( 'NONE',  ( 23.91535545868163126, 8.768263569673496960, -3.395287945660274254 ) ) ;
#10897 = VECTOR ( 'NONE', #11986, 1000.000000000000000 ) ;
#10898 = VERTEX_POINT ( 'NONE', #5705 ) ;
#10899 = CARTESIAN_POINT ( 'NONE',  ( 19.34511922692029984, 0.3276742896394955196, -15.04744788783380827 ) ) ;
#10900 = ADVANCED_FACE ( 'NONE', ( #2717 ), #19296, .T. ) ;
#10901 = CARTESIAN_POINT ( 'NONE',  ( 0.02681165389613587163, 15.20991100934055851, 0.9596687688324064824 ) ) ;
#10902 = EDGE_CURVE ( 'NONE', #2714, #2722, #12622, .T. ) ;
#10903 = ADVANCED_FACE ( 'NONE', ( #2277 ), #7474, .T. ) ;
#10904 = CARTESIAN_POINT ( 'NONE',  ( 11.60664369415897568, -3.109370887057594235, -16.86713491734067460 ) ) ;
#10905 = ORIENTED_EDGE ( 'NONE', *, *, #19853, .T. ) ;
#10906 = CARTESIAN_POINT ( 'NONE',  ( 29.76562500000000000, 0.000000000000000000, -4.317999999999999616 ) ) ;
#10907 = CIRCLE ( 'NONE', #1359, 0.7950200000000000600 ) ;
#10908 = CARTESIAN_POINT ( 'NONE',  ( 10.06470537354537242, 20.90551644660764197, -1.710021108312257176 ) ) ;
#10909 = CYLINDRICAL_SURFACE ( 'NONE', #18448, 9.524999999999998579 ) ;
#10910 = DIRECTION ( 'NONE',  ( 0.000000000000000000, -1.000000000000000000, 0.000000000000000000 ) ) ;
#10911 = CIRCLE ( 'NONE', #1371, 0.7950200000000000600 ) ;
#10912 = EDGE_LOOP ( 'NONE', ( #2948, #13948, #8419, #8169 ) ) ;
#10913 = CARTESIAN_POINT ( 'NONE',  ( -17.46249999999999858, -0.3962399999999990929, 0.000000000000000000 ) ) ;
#10915 = LINE ( 'NONE', #2513, #5216 ) ;
#10914 = CARTESIAN_POINT ( 'NONE',  ( 19.67909734877197891, 0.1298811790940870847, -14.89708569419555317 ) ) ;
#10916 = VERTEX_POINT ( 'NONE', #6138 ) ;
#10917 = VERTEX_POINT ( 'NONE', #17648 ) ;
#10918 = CARTESIAN_POINT ( 'NONE',  ( 11.44554379814851508, -6.402327797446566215, -17.01165796439540756 ) ) ;
#10920 = CARTESIAN_POINT ( 'NONE',  ( 31.83819605565793509, -3.968114999999999615, -4.158220719828246814 ) ) ;
#10919 = CARTESIAN_POINT ( 'NONE',  ( 5.658689206670286964, 21.64257598718208442, 3.780371088097784771 ) ) ;
#10921 = ORIENTED_EDGE ( 'NONE', *, *, #8673, .T. ) ;
#10922 = CARTESIAN_POINT ( 'NONE',  ( 3.524570301996365007, 14.53812262783368148, -1.106616872351161796 ) ) ;
#10923 = ORIENTED_EDGE ( 'NONE', *, *, #4372, .T. ) ;
#10924 = EDGE_LOOP ( 'NONE', ( #21072, #21003, #10155, #12616 ) ) ;
#10925 = EDGE_CURVE ( 'NONE', #3091, #20317, #16571, .T. ) ;
#10926 = AXIS2_PLACEMENT_3D ( 'NONE', #20718, #2267, #5572 ) ;
#10927 = VERTEX_POINT ( 'NONE', #9232 ) ;
#10928 = DIRECTION ( 'NONE',  ( 0.8609107660235850723, 0.000000000000000000, -0.5087559856598092844 ) ) ;
#10929 = AXIS2_PLACEMENT_3D ( 'NONE', #21116, #9725, #19576 ) ;
#10930 = DIRECTION ( 'NONE',  ( 0.000000000000000000, 1.000000000000000000, 0.000000000000000000 ) ) ;
#10931 = DIRECTION ( 'NONE',  ( 0.9959941601142464629, 0.000000000000000000, 0.08941830359784717908 ) ) ;
#10932 = CARTESIAN_POINT ( 'NONE',  ( 2.744809781688229311, 11.26550662193089991, 4.638685792162725363 ) ) ;
#10933 = ORIENTED_EDGE ( 'NONE', *, *, #5621, .T. ) ;
#10934 = CARTESIAN_POINT ( 'NONE',  ( 6.585898268469219552, 32.54502000000000095, 4.694966092919240275 ) ) ;
#10935 = DIRECTION ( 'NONE',  ( 1.000000000000000000, 0.000000000000000000, 0.000000000000000000 ) ) ;
#10936 = VERTEX_POINT ( 'NONE', #12676 ) ;
#10937 = ORIENTED_EDGE ( 'NONE', *, *, #21306, .F. ) ;
#10938 = CARTESIAN_POINT ( 'NONE',  ( 9.886113621169860366, 10.85891277430018143, 2.317410492099426289 ) ) ;
#10939 = VECTOR ( 'NONE', #13766, 1000.000000000000000 ) ;
#10941 = DIRECTION ( 'NONE',  ( 0.1060008583745200711, 0.000000000000000000, 0.9943660382494290406 ) ) ;
#10940 = DIRECTION ( 'NONE',  ( 0.2490110332224846346, 0.000000000000000000, -0.9685006480810792739 ) ) ;
#10942 = CARTESIAN_POINT ( 'NONE',  ( 11.93614680372799164, 10.48196076179804237, 0.4944231461740059563 ) ) ;
#10943 = ORIENTED_EDGE ( 'NONE', *, *, #21018, .F. ) ;
#10944 = EDGE_LOOP ( 'NONE', ( #9379, #20073, #17255, #2046 ) ) ;
#10945 = CARTESIAN_POINT ( 'NONE',  ( 61.09555596642878328, 0.000000000000000000, -12.53419992421059348 ) ) ;
#10946 = CARTESIAN_POINT ( 'NONE',  ( 7.422254420035173439, 12.63626090060510165, -1.507133129890835477 ) ) ;
#10947 = DIRECTION ( 'NONE',  ( 0.000000000000000000, -1.000000000000000000, 0.000000000000000000 ) ) ;
#10948 = DIRECTION ( 'NONE',  ( -0.08420877549337300871, 0.000000000000000000, -0.9964481331860212121 ) ) ;
#10949 = CIRCLE ( 'NONE', #17291, 2.182812499999999378 ) ;
#10950 = CIRCLE ( 'NONE', #1409, 5.357812499999999645 ) ;
#10951 = CARTESIAN_POINT ( 'NONE',  ( 7.677630431870579031, 20.85973498604326082, 3.570432132007519410 ) ) ;
#10952 = CARTESIAN_POINT ( 'NONE',  ( 7.313927782523842680, 14.57437388699512049, 7.297072825503160942 ) ) ;
#10953 = EDGE_CURVE ( 'NONE', #395, #12583, #16012, .T. ) ;
#10954 = CARTESIAN_POINT ( 'NONE',  ( 2.405822869029970335, 19.95883502769006768, 6.363079012132137890 ) ) ;
#10955 = DIRECTION ( 'NONE',  ( 0.000000000000000000, -1.000000000000000000, 0.000000000000000000 ) ) ;
#10956 = DIRECTION ( 'NONE',  ( -0.9685006480810794960, 0.000000000000000000, -0.2490110332224836354 ) ) ;
#10957 = AXIS2_PLACEMENT_3D ( 'NONE', #20892, #4534, #12518 ) ;
#10958 = CARTESIAN_POINT ( 'NONE',  ( 5.749403582042253547, 12.07884102837326168, -0.3386244590164438351 ) ) ;
#10959 = LINE ( 'NONE', #12631, #2622 ) ;
#10960 = DIRECTION ( 'NONE',  ( 0.2490110332224846623, 0.000000000000000000, -0.9685006480810793850 ) ) ;
#10961 = CARTESIAN_POINT ( 'NONE',  ( -0.9269672813091816010, 20.56277232864792026, 3.255889307845898806 ) ) ;
#10962 = CARTESIAN_POINT ( 'NONE',  ( 0.3520923380729273355, 20.79332306228696226, 6.585738808535214872 ) ) ;
#10963 = CARTESIAN_POINT ( 'NONE',  ( 2.492193568723835462, 25.39269750000000059, -24.56873394466936134 ) ) ;
#10964 = VECTOR ( 'NONE', #17272, 1000.000000000000000 ) ;
#10965 = CARTESIAN_POINT ( 'NONE',  ( 2.898989268417691889, 20.19932627889173915, 2.190770615898228968 ) ) ;
#10966 = FACE_BOUND ( 'NONE', #3829, .T. ) ;
#10967 = CARTESIAN_POINT ( 'NONE',  ( 19.64230669971109222, 0.5287862484321461665, -14.36345453931188665 ) ) ;
#10968 = AXIS2_PLACEMENT_3D ( 'NONE', #4695, #1581, #19931 ) ;
#10969 = ORIENTED_EDGE ( 'NONE', *, *, #17925, .F. ) ;
#10970 = DIRECTION ( 'NONE',  ( -0.2868778675745010664, 0.000000000000000000, -0.9579671649362032637 ) ) ;
#10971 = CARTESIAN_POINT ( 'NONE',  ( 10.99108388080240850, 11.53754468935924216, 5.084071353150248385 ) ) ;
#10972 = EDGE_LOOP ( 'NONE', ( #15723, #866, #21740, #20527, #10602, #19216 ) ) ;
#10973 = EDGE_CURVE ( 'NONE', #2204, #6418, #5597, .T. ) ;
#10974 = CARTESIAN_POINT ( 'NONE',  ( 28.78027906680959802, 1.604082891229885011, 10.67911709002892096 ) ) ;
#10975 = AXIS2_PLACEMENT_3D ( 'NONE', #18021, #15951, #2552 ) ;
#10976 = CARTESIAN_POINT ( 'NONE',  ( 5.387739448560934896, 14.30193700830310277, -1.760619005860999398 ) ) ;
#10977 = CARTESIAN_POINT ( 'NONE',  ( 1.998220421679061776, 25.39269750000000059, -22.64748046904500356 ) ) ;
#10978 = AXIS2_PLACEMENT_3D ( 'NONE', #13572, #5147, #10231 ) ;
#10979 = ORIENTED_EDGE ( 'NONE', *, *, #7537, .F. ) ;
#10980 = EDGE_CURVE ( 'NONE', #7865, #17422, #16558, .T. ) ;
#10981 = ADVANCED_FACE ( 'NONE', ( #21167 ), #6022, .T. ) ;
#10982 = DIRECTION ( 'NONE',  ( 0.7421532822901579785, 0.000000000000000000, -0.6702301885068628895 ) ) ;
#10983 = EDGE_LOOP ( 'NONE', ( #10367, #987, #8490, #3729 ) ) ;
#10984 = CARTESIAN_POINT ( 'NONE',  ( 11.23558539073912499, 16.27078549497860394, -3.718151546694987708 ) ) ;
#10985 = PRESENTATION_LAYER_ASSIGNMENT (  '', '', ( #2514 ) ) ;
#10986 = CARTESIAN_POINT ( 'NONE',  ( 11.33660541269852295, 21.35754284105190237, 1.979928130275292020 ) ) ;
#10987 = CARTESIAN_POINT ( 'NONE',  ( 41.78116128337411794, -1.983739999999999837, 7.392073290253172502 ) ) ;
#10988 = AXIS2_PLACEMENT_3D ( 'NONE', #8111, #16438, #4384 ) ;
#10989 = CIRCLE ( 'NONE', #2110, 0.5080000000000013394 ) ;
#10990 = CARTESIAN_POINT ( 'NONE',  ( 41.45112526417833010, 32.54502000000000095, 7.778260066349530710 ) ) ;
#10991 = CARTESIAN_POINT ( 'NONE',  ( 64.19677489640052670, -4.569743463999999200, -11.74367670905533423 ) ) ;
#10992 = CARTESIAN_POINT ( 'NONE',  ( 4.104248940463866013, 21.17924991814257396, 5.336610038632097819 ) ) ;
#10993 = PRODUCT_DEFINITION_CONTEXT ( 'detailed design', #983, 'design' ) ;
#10994 = CARTESIAN_POINT ( 'NONE',  ( 61.02111788801703085, -1.983739999999999837, -5.406220493519755088 ) ) ;
#10995 = VERTEX_POINT ( 'NONE', #4385 ) ;
#10996 = ADVANCED_FACE ( 'NONE', ( #1049 ), #4487, .T. ) ;
#10997 = LINE ( 'NONE', #9107, #20428 ) ;
#10998 = ORIENTED_EDGE ( 'NONE', *, *, #9921, .F. ) ;
#10999 = CARTESIAN_POINT ( 'NONE',  ( 10.66809636617878532, 20.98977402726757902, 0.2570665557559146386 ) ) ;
#11000 = DIRECTION ( 'NONE',  ( 0.8334497143791951279, 0.000000000000000000, 0.5525953072558960066 ) ) ;
#11001 = CARTESIAN_POINT ( 'NONE',  ( 42.94469661997857912, -76.79125307200000350, -18.48251861828712705 ) ) ;
#11003 = CARTESIAN_POINT ( 'NONE',  ( 9.256853431388732290, -3.968114999999999615, -17.09316853730597074 ) ) ;
#11002 = CARTESIAN_POINT ( 'NONE',  ( 1.191453932260699400, 15.64505045901557345, 9.398635499751998523 ) ) ;
#11004 = ORIENTED_EDGE ( 'NONE', *, *, #15072, .T. ) ;
#11005 = FACE_BOUND ( 'NONE', #10656, .T. ) ;
#11006 = VECTOR ( 'NONE', #21035, 1000.000000000000000 ) ;
#11007 = CARTESIAN_POINT ( 'NONE',  ( 39.18191486213413555, -5.198066315796270764, -3.704589387597398087 ) ) ;
#11008 = AXIS2_PLACEMENT_3D ( 'NONE', #1442, #4662, #21678 ) ;
#11009 = AXIS2_PLACEMENT_3D ( 'NONE', #1610, #11790, #3388 ) ;
#11010 = ORIENTED_EDGE ( 'NONE', *, *, #8390, .T. ) ;
#11011 = EDGE_CURVE ( 'NONE', #14493, #14322, #3149, .T. ) ;
#11012 = CARTESIAN_POINT ( 'NONE',  ( 49.16323787629939801, -42.42568807200000691, -27.09503225884920141 ) ) ;
#11013 = AXIS2_PLACEMENT_3D ( 'NONE', #3433, #10168, #8503 ) ;
#11014 = CARTESIAN_POINT ( 'NONE',  ( 19.42050984830941829, -5.834154119974274799, -15.51764488770388972 ) ) ;
#11015 = VERTEX_POINT ( 'NONE', #9772 ) ;
#11016 = DIRECTION ( 'NONE',  ( 0.000000000000000000, -1.000000000000000000, 0.000000000000000000 ) ) ;
#11017 = EDGE_CURVE ( 'NONE', #6939, #7791, #9873, .T. ) ;
#11018 = SHAPE_REPRESENTATION ( 'Frame Locking Pawl Plate', ( #2234 ), #10885 ) ;
#11019 = AXIS2_PLACEMENT_3D ( 'NONE', #17239, #7615, #5940 ) ;
#11020 = DIRECTION ( 'NONE',  ( 0.000000000000000000, 1.000000000000000000, 0.000000000000000000 ) ) ;
#11021 = VECTOR ( 'NONE', #4751, 1000.000000000000000 ) ;
#11022 = ORIENTED_EDGE ( 'NONE', *, *, #14572, .F. ) ;
#11023 = CARTESIAN_POINT ( 'NONE',  ( -12.30312499999999964, 2.380615000000000148, 8.335010000000000474 ) ) ;
#11024 = EDGE_CURVE ( 'NONE', #17175, #1068, #15006, .T. ) ;
#11026 = CARTESIAN_POINT ( 'NONE',  ( 10.10534066920194185, -3.968114999999999615, -14.00784516691476966 ) ) ;
#11025 = CARTESIAN_POINT ( 'NONE',  ( 42.79471501377724252, 0.000000000000000000, 5.049205022181460834 ) ) ;
#11027 = ORIENTED_EDGE ( 'NONE', *, *, #21423, .F. ) ;
#11028 = EDGE_CURVE ( 'NONE', #18192, #12175, #16539, .T. ) ;
#11029 = VERTEX_POINT ( 'NONE', #21723 ) ;
#11030 = CIRCLE ( 'NONE', #3611, 1.190625000000001155 ) ;
#11031 = AXIS2_PLACEMENT_3D ( 'NONE', #9435, #3133, #1032 ) ;
#11033 = DIRECTION ( 'NONE',  ( -0.8943161143440100380, 0.000000000000000000, -0.4474356798743607255 ) ) ;
#11032 = CARTESIAN_POINT ( 'NONE',  ( 3.559759918315169358, 13.11356558266398231, 8.212977649209914688 ) ) ;
#11034 = EDGE_LOOP ( 'NONE', ( #889, #7929, #11467, #17458 ) ) ;
#11035 = CARTESIAN_POINT ( 'NONE',  ( 3.568439739289405388, 16.69396391803602953, -1.421120065001460153 ) ) ;
#11036 = ORIENTED_EDGE ( 'NONE', *, *, #3794, .F. ) ;
#11037 = ORIENTED_EDGE ( 'NONE', *, *, #8070, .T. ) ;
#11038 = VECTOR ( 'NONE', #2507, 1000.000000000000000 ) ;
#11039 = EDGE_LOOP ( 'NONE', ( #5946, #4178, #8362, #19372 ) ) ;
#11040 = CARTESIAN_POINT ( 'NONE',  ( 3.133115509155857570, 12.68908857082841735, 6.468163464435182419 ) ) ;
#11041 = AXIS2_PLACEMENT_3D ( 'NONE', #14994, #21711, #4582 ) ;
#11042 = STYLED_ITEM ( 'NONE', ( #2756 ), #21013 ) ;
#11043 = CARTESIAN_POINT ( 'NONE',  ( 71.04062499999999147, 0.000000000000000000, -10.31874999999999964 ) ) ;
#11044 = FACE_OUTER_BOUND ( 'NONE', #11878, .T. ) ;
#11045 = CARTESIAN_POINT ( 'NONE',  ( 46.03750000000000142, 36.51313500000000545, -10.31874999999999964 ) ) ;
#11046 = DIRECTION ( 'NONE',  ( -0.2868778675745011220, 0.000000000000000000, -0.9579671649362034858 ) ) ;
#11047 = CARTESIAN_POINT ( 'NONE',  ( 3.649632197277235424, 15.51727318038290626, 9.145577215261649684 ) ) ;
#11048 = ORIENTED_EDGE ( 'NONE', *, *, #7340, .T. ) ;
#11049 = CARTESIAN_POINT ( 'NONE',  ( 38.82016491058538321, -1.983739999999999837, -14.75770094105646812 ) ) ;
#11050 = DIRECTION ( 'NONE',  ( 0.9685006480810790519, 0.000000000000000000, 0.2490110332224857170 ) ) ;
#11051 = FACE_OUTER_BOUND ( 'NONE', #11484, .T. ) ;
#11052 = FILL_AREA_STYLE_COLOUR ( '', #13894 ) ;
#11053 = VECTOR ( 'NONE', #14821, 1000.000000000000000 ) ;
#11054 = ORIENTED_EDGE ( 'NONE', *, *, #18177, .T. ) ;
#11055 = EDGE_CURVE ( 'NONE', #1512, #968, #2824, .T. ) ;
#11056 = ORIENTED_EDGE ( 'NONE', *, *, #17146, .T. ) ;
#11057 = CARTESIAN_POINT ( 'NONE',  ( 6.326270045413027177, 11.43880029099476126, 4.501843889239982133 ) ) ;
#11059 = DIRECTION ( 'NONE',  ( 0.000000000000000000, 1.000000000000000000, 0.000000000000000000 ) ) ;
#11058 = DIRECTION ( 'NONE',  ( 0.000000000000000000, 1.000000000000000000, 0.000000000000000000 ) ) ;
#11060 = CARTESIAN_POINT ( 'NONE',  ( 13.34474349389573966, 13.82947554229071585, 6.637995438756325584 ) ) ;
#11061 = ORIENTED_EDGE ( 'NONE', *, *, #19696, .F. ) ;
#11062 = ORIENTED_EDGE ( 'NONE', *, *, #11801, .T. ) ;
#11063 = DIRECTION ( 'NONE',  ( 0.000000000000000000, -1.000000000000000000, -0.000000000000000000 ) ) ;
#11064 = CARTESIAN_POINT ( 'NONE',  ( 7.899748338964175609, 11.10891229026089988, 0.6199817720100504470 ) ) ;
#11065 = CIRCLE ( 'NONE', #6099, 3.968750000000000000 ) ;
#11066 = CARTESIAN_POINT ( 'NONE',  ( 1.994785678335496026, 13.53119643653954363, 0.9820674903561780189 ) ) ;
#11067 = CARTESIAN_POINT ( 'NONE',  ( 7.505597285291182530, 20.91029632882624156, 3.112204859505360410 ) ) ;
#11068 = CARTESIAN_POINT ( 'NONE',  ( 7.235830445973447489, 13.61491138090174680, 6.770065179283416334 ) ) ;
#11069 = CARTESIAN_POINT ( 'NONE',  ( 2.011838081192605987, 20.33402069578789551, 5.352005239497477085 ) ) ;
#11070 = CARTESIAN_POINT ( 'NONE',  ( 15.47835459351327714, -5.959792500000001603, 5.813316144137728791 ) ) ;
#11071 = VECTOR ( 'NONE', #11428, 1000.000000000000000 ) ;
#11072 = FACE_OUTER_BOUND ( 'NONE', #15555, .T. ) ;
#11073 = CARTESIAN_POINT ( 'NONE',  ( 8.251602663485694933, 10.68384337266676276, 1.704364278152144196 ) ) ;
#11074 = CARTESIAN_POINT ( 'NONE',  ( 56.47666780297049627, -1.983739999999999393, 1.109116340531466127 ) ) ;
#11075 = CARTESIAN_POINT ( 'NONE',  ( -23.01875000000000071, 32.54502000000000095, -10.31874999999999964 ) ) ;
#11076 = CARTESIAN_POINT ( 'NONE',  ( 0.1889641725767322034, 19.02238102577908307, 0.6697343601325994600 ) ) ;
#11077 = CARTESIAN_POINT ( 'NONE',  ( 1.640147784336999592, 16.65909851697077571, 9.606380118624771924 ) ) ;
#11078 = AXIS2_PLACEMENT_3D ( 'NONE', #14401, #10955, #4937 ) ;
#11079 = CARTESIAN_POINT ( 'NONE',  ( 46.03750000000000142, -14.84248999999999974, -10.31874999999999964 ) ) ;
#11080 = CARTESIAN_POINT ( 'NONE',  ( 5.376211239829841837, 15.73786965665290793, 8.095709214974558421 ) ) ;
#11081 = CARTESIAN_POINT ( 'NONE',  ( 1.268730000000000135, 23.41816500000000190, 10.65596716962832069 ) ) ;
#11082 = FACE_OUTER_BOUND ( 'NONE', #12227, .T. ) ;
#11083 = CARTESIAN_POINT ( 'NONE',  ( 14.89546171155516063, -8.373827889660200086, -15.10229938975829178 ) ) ;
#11084 = VERTEX_POINT ( 'NONE', #21611 ) ;
#11085 = CARTESIAN_POINT ( 'NONE',  ( 53.00421038040393995, 29.95901653600000003, 6.511420152579801446 ) ) ;
#11086 = EDGE_CURVE ( 'NONE', #21183, #20725, #16326, .T. ) ;
#11087 = CARTESIAN_POINT ( 'NONE',  ( 10.81776401011329547, 11.10301140953592203, 4.334198581180471521 ) ) ;
#11088 = ORIENTED_EDGE ( 'NONE', *, *, #11108, .F. ) ;
#11089 = CIRCLE ( 'NONE', #1544, 0.7950199999999982836 ) ;
#11090 = LINE ( 'NONE', #9526, #20163 ) ;
#11091 = CARTESIAN_POINT ( 'NONE',  ( 12.16036747447985711, 20.61529458018329564, -1.409506725801037419 ) ) ;
#11092 = CARTESIAN_POINT ( 'NONE',  ( 5.483538033079329743, 13.23206236587151707, -1.192467485947962036 ) ) ;
#11093 = DIRECTION ( 'NONE',  ( 0.000000000000000000, -1.000000000000000000, 0.000000000000000000 ) ) ;
#11094 = CARTESIAN_POINT ( 'NONE',  ( 1.113804815293770289, 18.49964734577863368, 8.330481410010762033 ) ) ;
#11095 = ORIENTED_EDGE ( 'NONE', *, *, #13204, .T. ) ;
#11096 = DIRECTION ( 'NONE',  ( 1.000000000000000000, 0.000000000000000000, 0.000000000000000000 ) ) ;
#11097 = AXIS2_PLACEMENT_3D ( 'NONE', #19674, #21441, #6299 ) ;
#11098 = CARTESIAN_POINT ( 'NONE',  ( 7.134758565295798327, 11.94621801824261986, 4.715951947576552783 ) ) ;
#11099 = CIRCLE ( 'NONE', #6507, 1.785937499999999956 ) ;
#11100 = FACE_OUTER_BOUND ( 'NONE', #18712, .T. ) ;
#11101 = CARTESIAN_POINT ( 'NONE',  ( 65.51436440461340283, 30.56064500000000095, -12.87863775929475985 ) ) ;
#11102 = CARTESIAN_POINT ( 'NONE',  ( 39.07078961959606289, 29.95901653600000003, -27.14892015257980162 ) ) ;
#11103 = CARTESIAN_POINT ( 'NONE',  ( 3.697979674205963185, 21.37068642827637888, 4.236069647309165020 ) ) ;
#11104 = LINE ( 'NONE', #12449, #14524 ) ;
#11105 = ADVANCED_FACE ( 'NONE', ( #8759 ), #18608, .T. ) ;
#11106 = ORIENTED_EDGE ( 'NONE', *, *, #19747, .F. ) ;
#11107 = CARTESIAN_POINT ( 'NONE',  ( -14.90829243662478909, 34.62011481965967619, -10.03143607188557418 ) ) ;
#11108 = EDGE_CURVE ( 'NONE', #5953, #19328, #259, .T. ) ;
#11109 = VECTOR ( 'NONE', #15301, 1000.000000000000114 ) ;
#11110 = DIRECTION ( 'NONE',  ( 0.000000000000000000, -1.000000000000000000, -0.000000000000000000 ) ) ;
#11111 = ORIENTED_EDGE ( 'NONE', *, *, #8070, .F. ) ;
#11112 = CARTESIAN_POINT ( 'NONE',  ( 11.36271039377850300, 21.23937884529802389, 2.129853413371744164 ) ) ;
#11113 = CARTESIAN_POINT ( 'NONE',  ( 1.467157081727171297, 15.86225324810530068, 8.827709964917746177 ) ) ;
#11114 = CARTESIAN_POINT ( 'NONE',  ( 17.12871318600645409, 2.301163489826294484, -14.63919962258086827 ) ) ;
#11116 = LINE ( 'NONE', #10893, #21224 ) ;
#11115 = CARTESIAN_POINT ( 'NONE',  ( 1.328448286825129943, 14.75527451915623267, -0.007290130677178787572 ) ) ;
#11117 = ORIENTED_EDGE ( 'NONE', *, *, #15060, .F. ) ;
#11118 = CIRCLE ( 'NONE', #1574, 1.190624999999997824 ) ;
#11119 = PLANE ( 'NONE',  #7452 ) ;
#11120 = CARTESIAN_POINT ( 'NONE',  ( 39.38402901577369875, -5.317104264161899074, -3.501309714141658258 ) ) ;
#11121 = ORIENTED_EDGE ( 'NONE', *, *, #16533, .F. ) ;
#11122 = CARTESIAN_POINT ( 'NONE',  ( 19.98142615554668566, -0.9834789709510379785, -14.83023175912481051 ) ) ;
#11123 = CARTESIAN_POINT ( 'NONE',  ( 19.93414139600567125, -1.593704270021353953, -15.40834236525699730 ) ) ;
#11124 = ORIENTED_EDGE ( 'NONE', *, *, #20699, .T. ) ;
#11125 = CARTESIAN_POINT ( 'NONE',  ( 10.09152440736383483, 20.26472116815758184, -1.194358939805918896 ) ) ;
#11126 = ADVANCED_FACE ( 'NONE', ( #10209 ), #13769, .T. ) ;
#11127 = CARTESIAN_POINT ( 'NONE',  ( 20.23508918937977796, -1.359453322992689506, -14.75410208910826704 ) ) ;
#11128 = CARTESIAN_POINT ( 'NONE',  ( 7.185023862866797728, 14.38088390058819144, -2.647084244243658624 ) ) ;
#11129 = VECTOR ( 'NONE', #6717, 1000.000000000000000 ) ;
#11130 = PLANE ( 'NONE',  #12273 ) ;
#11131 = EDGE_CURVE ( 'NONE', #5927, #14184, #3375, .T. ) ;
#11132 = ORIENTED_EDGE ( 'NONE', *, *, #10338, .T. ) ;
#11133 = EDGE_CURVE ( 'NONE', #1512, #7380, #16953, .T. ) ;
#11134 = DIRECTION ( 'NONE',  ( -0.9790635044817342925, 0.000000000000000000, 0.2035550397114870846 ) ) ;
#11136 = DIRECTION ( 'NONE',  ( 0.000000000000000000, -1.000000000000000000, 0.000000000000000000 ) ) ;
#11135 = CARTESIAN_POINT ( 'NONE',  ( 8.505511374756364873, 24.59767750000000319, -20.97439202360551747 ) ) ;
#11137 = ORIENTED_EDGE ( 'NONE', *, *, #2372, .T. ) ;
#11138 = ORIENTED_EDGE ( 'NONE', *, *, #16446, .T. ) ;
#11139 = CARTESIAN_POINT ( 'NONE',  ( 17.52996087073869447, -8.549669343631473239, -15.68810240790472577 ) ) ;
#11141 = DIRECTION ( 'NONE',  ( -0.000000000000000000, -1.000000000000000000, 0.000000000000000000 ) ) ;
#11140 = CARTESIAN_POINT ( 'NONE',  ( 5.642613892620969018, 15.64107961637180289, 8.855653260751193301 ) ) ;
#11142 = VERTEX_POINT ( 'NONE', #8432 ) ;
#11143 = CARTESIAN_POINT ( 'NONE',  ( 4.143869576618084416, 19.77995523304069181, -0.2166999831453354231 ) ) ;
#11144 = VERTEX_POINT ( 'NONE', #17068 ) ;
#11145 = ORIENTED_EDGE ( 'NONE', *, *, #7461, .F. ) ;
#11146 = CIRCLE ( 'NONE', #1603, 0.5080000000000000071 ) ;
#11147 = SHAPE_REPRESENTATION ( 'Handle Pawl Torsion Spring', ( #2234 ), #4182 ) ;
#11148 = EDGE_LOOP ( 'NONE', ( #5877, #19103, #2503, #14349, #14887, #13963, #6694, #4758, #2787, #6455, #17476, #8280, #1638, #8606, #16123, #9531, #4450, #10349, #779, #20739, #13058 ) ) ;
#11149 = EDGE_CURVE ( 'NONE', #13907, #13654, #7718, .T. ) ;
#11150 = CARTESIAN_POINT ( 'NONE',  ( 7.241402720468077092, 25.39269750000000059, -19.25049230170216319 ) ) ;
#11151 = CARTESIAN_POINT ( 'NONE',  ( -47.86049599909252805, -8.889364999999999739, -23.29373766372935961 ) ) ;
#11152 = LINE ( 'NONE', #12940, #7917 ) ;
#11153 = CARTESIAN_POINT ( 'NONE',  ( -13.97426865170217702, 38.49878000000000355, -10.62412961436650249 ) ) ;
#11154 = EDGE_LOOP ( 'NONE', ( #4711, #412, #18509, #9579 ) ) ;
#11155 = DIRECTION ( 'NONE',  ( 0.6702301885068638887, 0.000000000000000000, 0.7421532822901570903 ) ) ;
#11156 = DIRECTION ( 'NONE',  ( 0.000000000000000000, -1.000000000000000000, -0.000000000000000000 ) ) ;
#11157 = DIRECTION ( 'NONE',  ( 0.9564948366894089338, -0.05542109139015086172, -0.2864369564417716951 ) ) ;
#11158 = CARTESIAN_POINT ( 'NONE',  ( 28.87608719841374949, 40.07707250000000698, -15.73691681567849976 ) ) ;
#11159 = DIRECTION ( 'NONE',  ( -0.2490110332224836354, 0.000000000000000000, 0.9685006480810794960 ) ) ;
#11160 = VERTEX_POINT ( 'NONE', #10440 ) ;
#11161 = ORIENTED_EDGE ( 'NONE', *, *, #9890, .T. ) ;
#11162 = CARTESIAN_POINT ( 'NONE',  ( 5.810800753368915217, 11.79079236785502260, 1.673948637325690880 ) ) ;
#11164 = DIRECTION ( 'NONE',  ( 0.9685006480810791629, 0.000000000000000000, 0.2490110332224850231 ) ) ;
#11163 = DIRECTION ( 'NONE',  ( -1.000000000000000000, 0.000000000000000000, 0.000000000000000000 ) ) ;
#11165 = CARTESIAN_POINT ( 'NONE',  ( 11.92791153145151739, 21.07569174392700262, -2.114904552164332152 ) ) ;
#11166 = EDGE_LOOP ( 'NONE', ( #18415, #5936, #8428, #8249, #2638, #9321 ) ) ;
#11167 = ORIENTED_EDGE ( 'NONE', *, *, #11524, .F. ) ;
#11168 = DIRECTION ( 'NONE',  ( -0.000000000000000000, -1.000000000000000000, 0.000000000000000000 ) ) ;
#11169 = CARTESIAN_POINT ( 'NONE',  ( 8.438110056274945592, 21.24481177138277133, -0.1056387872616715573 ) ) ;
#11170 = CARTESIAN_POINT ( 'NONE',  ( 7.534092756634481525, 20.90493591499421200, 3.188157648738980221 ) ) ;
#11171 = CARTESIAN_POINT ( 'NONE',  ( 2.836490765739545061, 19.10541491058949148, 7.422640015091157117 ) ) ;
#11172 = EDGE_CURVE ( 'NONE', #19449, #14145, #13548, .T. ) ;
#11173 = EDGE_CURVE ( 'NONE', #21060, #16032, #11607, .T. ) ;
#11174 = CARTESIAN_POINT ( 'NONE',  ( 24.26606285357373594, 28.96330250000000461, -16.92219937337620195 ) ) ;
#11175 = CARTESIAN_POINT ( 'NONE',  ( 5.422126241162127158, 15.44426253303012508, -2.220568121751542279 ) ) ;
#11176 = CARTESIAN_POINT ( 'NONE',  ( 13.75503787843007153, 21.87849604123467628, 1.799798963432884813 ) ) ;
#11177 = DIRECTION ( 'NONE',  ( 0.000000000000000000, -1.000000000000000000, -0.000000000000000000 ) ) ;
#11178 = CARTESIAN_POINT ( 'NONE',  ( 5.614158541085368270, 21.64188095357850372, 3.793657251346655990 ) ) ;
#11179 = CARTESIAN_POINT ( 'NONE',  ( 1.652283335345338333, 13.93189131863066166, 9.000229686725790046 ) ) ;
#11180 = AXIS2_PLACEMENT_3D ( 'NONE', #18493, #3254, #10428 ) ;
#11181 = ORIENTED_EDGE ( 'NONE', *, *, #14170, .T. ) ;
#11182 = CARTESIAN_POINT ( 'NONE',  ( 0.2271524594679337483, 17.19594618500607908, 0.7656857658610515260 ) ) ;
#11183 = DIRECTION ( 'NONE',  ( 0.7532174416907910786, 0.000000000000000000, 0.6577716059034319773 ) ) ;
#11184 = FACE_OUTER_BOUND ( 'NONE', #17643, .T. ) ;
#11185 = CARTESIAN_POINT ( 'NONE',  ( 11.77191967066123723, -6.633846379865024012, -15.76999337786026345 ) ) ;
#11186 = ORIENTED_EDGE ( 'NONE', *, *, #592, .T. ) ;
#11187 = DIRECTION ( 'NONE',  ( -0.6702301885068628895, 0.000000000000000000, -0.7421532822901579785 ) ) ;
#11188 = CARTESIAN_POINT ( 'NONE',  ( 10.05023619051239692, 20.92035919996038018, -1.465514317523238352 ) ) ;
#11189 = ORIENTED_EDGE ( 'NONE', *, *, #19135, .F. ) ;
#11190 = CARTESIAN_POINT ( 'NONE',  ( 29.12736005702520359, 1.738817766846714852, 10.70064947183834114 ) ) ;
#11191 = CARTESIAN_POINT ( 'NONE',  ( 11.95168768794008152, 20.18527580681268319, -1.951704133241007444 ) ) ;
#11192 = CARTESIAN_POINT ( 'NONE',  ( 5.788809795094107535, 19.11881477019754172, -1.442269818482195154 ) ) ;
#11193 = CARTESIAN_POINT ( 'NONE',  ( 49.79678389823170903, -1.983739999999999837, -28.13445659451038594 ) ) ;
#11194 = CARTESIAN_POINT ( 'NONE',  ( 3.667426890329681832, 14.05442396375879710, -0.1080398768186726643 ) ) ;
#11195 = ORIENTED_EDGE ( 'NONE', *, *, #19050, .F. ) ;
#11196 = CYLINDRICAL_SURFACE ( 'NONE', #11695, 1.191259999999999319 ) ;
#11197 = CARTESIAN_POINT ( 'NONE',  ( 5.926337056667366099, 20.60626622430410038, 4.527039204987015175 ) ) ;
#11198 = FACE_OUTER_BOUND ( 'NONE', #14370, .T. ) ;
#11199 = ORIENTED_EDGE ( 'NONE', *, *, #286, .F. ) ;
#11200 = EDGE_CURVE ( 'NONE', #7817, #8399, #14092, .T. ) ;
#11201 = CARTESIAN_POINT ( 'NONE',  ( 11.39119446960197912, 12.85296284657052190, -2.409457258905069121 ) ) ;
#11202 = CARTESIAN_POINT ( 'NONE',  ( 5.036654803598190178, 18.32506955479991007, 7.572670103872398251 ) ) ;
#11203 = CARTESIAN_POINT ( 'NONE',  ( 28.56548256563643662, 34.52875999999999834, -12.12873025803960658 ) ) ;
#11204 = CARTESIAN_POINT ( 'NONE',  ( 38.27578610983103857, -5.744908453443699159, -4.797394063557049115 ) ) ;
#11205 = CARTESIAN_POINT ( 'NONE',  ( 1.687914040314732800, 17.33792227738861058, 9.588941613383601847 ) ) ;
#11206 = DIRECTION ( 'NONE',  ( 0.000000000000000000, 1.000000000000000000, 0.000000000000000000 ) ) ;
#11207 = DIRECTION ( 'NONE',  ( 0.000000000000000000, 1.000000000000000000, -0.000000000000000000 ) ) ;
#11208 = CARTESIAN_POINT ( 'NONE',  ( 20.53156541068710439, -1.359447366214681985, -15.90722246059563361 ) ) ;
#11209 = FACE_OUTER_BOUND ( 'NONE', #2752, .T. ) ;
#11210 = DIRECTION ( 'NONE',  ( -0.8609107660235850723, 0.000000000000000000, 0.5087559856598092844 ) ) ;
#11211 = VECTOR ( 'NONE', #17138, 1000.000000000000000 ) ;
#11212 = ORIENTED_EDGE ( 'NONE', *, *, #14399, .T. ) ;
#11213 = DIRECTION ( 'NONE',  ( 0.000000000000000000, 1.000000000000000000, 0.000000000000000000 ) ) ;
#11214 = FACE_OUTER_BOUND ( 'NONE', #7600, .T. ) ;
#11215 = EDGE_LOOP ( 'NONE', ( #14781, #8603, #23, #21764 ) ) ;
#11216 = CARTESIAN_POINT ( 'NONE',  ( 9.451771490251472230, 17.56608234664911450, -2.722081582746955775 ) ) ;
#11217 = CARTESIAN_POINT ( 'NONE',  ( 1.482573138264764223, 15.39360603941805294, 8.749273869541234205 ) ) ;
#11218 = CARTESIAN_POINT ( 'NONE',  ( 20.80998580648388341, -1.217322788665459177, -14.73620959842755695 ) ) ;
#11219 = DIRECTION ( 'NONE',  ( 0.1831666983862991482, 0.000000000000000000, -0.9830818687180954418 ) ) ;
#11220 = ORIENTED_EDGE ( 'NONE', *, *, #17206, .F. ) ;
#11221 = DIRECTION ( 'NONE',  ( -0.2490110332224850231, 0.000000000000000000, 0.9685006480810791629 ) ) ;
#11222 = DIRECTION ( 'NONE',  ( 0.000000000000000000, 1.000000000000000000, 0.000000000000000000 ) ) ;
#11223 = VERTEX_POINT ( 'NONE', #1914 ) ;
#11224 = CARTESIAN_POINT ( 'NONE',  ( 20.00345035822784467, -1.023028193093147076, -14.82316847688469785 ) ) ;
#11225 = EDGE_CURVE ( 'NONE', #15795, #15052, #296, .T. ) ;
#11226 = AXIS2_PLACEMENT_3D ( 'NONE', #7415, #17704, #10845 ) ;
#11227 = CARTESIAN_POINT ( 'NONE',  ( 12.11904762564861926, -6.033546283575153879, -17.57169469594360578 ) ) ;
#11228 = VERTEX_POINT ( 'NONE', #1334 ) ;
#11229 = CARTESIAN_POINT ( 'NONE',  ( 7.509149799818086279, 21.00645437613600208, 3.202027800742528463 ) ) ;
#11230 = CARTESIAN_POINT ( 'NONE',  ( 37.51913901087312553, 34.52875999999999834, -14.58057485080488114 ) ) ;
#11231 = CARTESIAN_POINT ( 'NONE',  ( 9.115559652288139247, 13.32446407270766287, -2.907578128373548232 ) ) ;
#11232 = CARTESIAN_POINT ( 'NONE',  ( 20.07818426912813337, -3.465737206707578011, -15.31859466601284403 ) ) ;
#11233 = CARTESIAN_POINT ( 'NONE',  ( 13.99260895880537525, 15.36419388438619649, -16.35910307397442054 ) ) ;
#11234 = ORIENTED_EDGE ( 'NONE', *, *, #7193, .F. ) ;
#11235 = CARTESIAN_POINT ( 'NONE',  ( 28.38195592936287781, 1.975802500000001904, -13.81504834214261024 ) ) ;
#11236 = CARTESIAN_POINT ( 'NONE',  ( -1.345424459097947834, 12.30439499999999953, 2.648158502653860324 ) ) ;
#11237 = VERTEX_POINT ( 'NONE', #11734 ) ;
#11238 = ORIENTED_EDGE ( 'NONE', *, *, #6431, .T. ) ;
#11239 = CIRCLE ( 'NONE', #10542, 1.785937499999999956 ) ;
#11240 = CARTESIAN_POINT ( 'NONE',  ( 21.27104401621292595, -2.646375628860768270, -13.78030298333726478 ) ) ;
#11242 = CYLINDRICAL_SURFACE ( 'NONE', #12035, 1.190625000000000711 ) ;
#11241 = CARTESIAN_POINT ( 'NONE',  ( 1.696449191584781024, 13.01816804744978207, 0.4119424741136656354 ) ) ;
#11243 = ORIENTED_EDGE ( 'NONE', *, *, #15074, .F. ) ;
#11244 = CARTESIAN_POINT ( 'NONE',  ( 4.268923416216722444, 20.13345205411175343, 0.09844701181663598200 ) ) ;
#11245 = EDGE_CURVE ( 'NONE', #7389, #12461, #6747, .T. ) ;
#11246 = ORIENTED_EDGE ( 'NONE', *, *, #14399, .F. ) ;
#11247 = VERTEX_POINT ( 'NONE', #20005 ) ;
#11248 = PRODUCT_DEFINITION_FORMATION_WITH_SPECIFIED_SOURCE ( 'ANY', '', #6509, .NOT_KNOWN. ) ;
#11249 = EDGE_CURVE ( 'NONE', #5690, #12990, #20780, .T. ) ;
#11250 = EDGE_LOOP ( 'NONE', ( #12932, #10260, #7577, #3644 ) ) ;
#11251 = EDGE_CURVE ( 'NONE', #16568, #3519, #4186, .T. ) ;
#11252 = AXIS2_PLACEMENT_3D ( 'NONE', #7026, #15684, #512 ) ;
#11253 = DIRECTION ( 'NONE',  ( 0.000000000000000000, 1.000000000000000000, 0.000000000000000000 ) ) ;
#11254 = CARTESIAN_POINT ( 'NONE',  ( 61.81956123787853130, -1.983739999999999837, -1.238102447480925239 ) ) ;
#11255 = DIRECTION ( 'NONE',  ( 0.8667647648559581031, 0.000000000000000000, 0.4987171968201974948 ) ) ;
#11256 = DIRECTION ( 'NONE',  ( 0.9685006480810794960, 0.000000000000000000, 0.2490110332224836354 ) ) ;
#11257 = CARTESIAN_POINT ( 'NONE',  ( 2.692116518274998427, 11.24804587133957234, 4.411506177232483061 ) ) ;
#11258 = ORIENTED_EDGE ( 'NONE', *, *, #21280, .F. ) ;
#11259 = DIRECTION ( 'NONE',  ( 0.000000000000000000, 1.000000000000000000, 0.000000000000000000 ) ) ;
#11260 = DIRECTION ( 'NONE',  ( 0.9784543669157944601, 0.000000000000000000, 0.2064631973582987667 ) ) ;
#11261 = CARTESIAN_POINT ( 'NONE',  ( -12.30312499999999964, 1.984057500000000251, 10.71562499999999929 ) ) ;
#11262 = LINE ( 'NONE', #9274, #19521 ) ;
#11263 = VECTOR ( 'NONE', #12098, 1000.000000000000000 ) ;
#11264 = CARTESIAN_POINT ( 'NONE',  ( 39.16413618835606769, 34.52875999999999834, -24.45043885672975392 ) ) ;
#11265 = ORIENTED_EDGE ( 'NONE', *, *, #261, .F. ) ;
#11266 = ORIENTED_EDGE ( 'NONE', *, *, #11017, .F. ) ;
#11267 = CARTESIAN_POINT ( 'NONE',  ( 5.240066203759783825, 15.55272378482423079, -1.415503761420363160 ) ) ;
#11269 = CARTESIAN_POINT ( 'NONE',  ( 59.65121809612895731, -1.983739999999999837, -2.485718937265306572 ) ) ;
#11268 = CYLINDRICAL_SURFACE ( 'NONE', #11890, 3.175000000000001155 ) ;
#11270 = CARTESIAN_POINT ( 'NONE',  ( 12.27216867080381313, 21.66113888363950224, -1.179511693193084465 ) ) ;
#11271 = ORIENTED_EDGE ( 'NONE', *, *, #2745, .F. ) ;
#11272 = EDGE_CURVE ( 'NONE', #12039, #18216, #15169, .T. ) ;
#11273 = ORIENTED_EDGE ( 'NONE', *, *, #20987, .T. ) ;
#11274 = CARTESIAN_POINT ( 'NONE',  ( 61.56621290189396944, -4.569743463999999200, -0.7977859469341201937 ) ) ;
#11275 = VECTOR ( 'NONE', #3630, 1000.000000000000000 ) ;
#11276 = CARTESIAN_POINT ( 'NONE',  ( 7.448527747198094850, 20.91460427354139995, 2.960036828183352231 ) ) ;
#11277 = CIRCLE ( 'NONE', #16921, 0.7950200000000010592 ) ;
#11278 = EDGE_CURVE ( 'NONE', #5733, #21341, #20059, .T. ) ;
#11279 = CARTESIAN_POINT ( 'NONE',  ( 3.045314960206396471, 18.44351948381887141, 7.897937509798712341 ) ) ;
#11280 = VECTOR ( 'NONE', #20017, 1000.000000000000114 ) ;
#11281 = CARTESIAN_POINT ( 'NONE',  ( 13.51968262288867884, 21.40970857061781274, 1.801479536130566661 ) ) ;
#11282 = CARTESIAN_POINT ( 'NONE',  ( -3.037751992662818257, 28.56769750000000130, -30.02724401157551526 ) ) ;
#11283 = DIRECTION ( 'NONE',  ( 0.000000000000000000, 1.000000000000000000, 0.000000000000000000 ) ) ;
#11284 = CARTESIAN_POINT ( 'NONE',  ( 0.3903923183617534765, 11.71055314899741084, 3.226328323983417068 ) ) ;
#11285 = DIRECTION ( 'NONE',  ( -0.3449240378348910063, 0.000000000000000000, 0.9386306025927743102 ) ) ;
#11286 = ORIENTED_EDGE ( 'NONE', *, *, #11430, .T. ) ;
#11287 = CARTESIAN_POINT ( 'NONE',  ( 4.511335975532223763, 19.89702943876222108, 0.8677524747804959970 ) ) ;
#11288 = CARTESIAN_POINT ( 'NONE',  ( 0.02083138522551555155, 20.24316500000000119, 7.210477125664100484 ) ) ;
#11289 = CARTESIAN_POINT ( 'NONE',  ( 21.03437500000000071, 32.54502000000000095, 5.159374999999999822 ) ) ;
#11290 = CARTESIAN_POINT ( 'NONE',  ( 20.65970833833902986, -4.825822034318000497, -13.89237661239871358 ) ) ;
#11291 = ORIENTED_EDGE ( 'NONE', *, *, #10578, .F. ) ;
#11292 = CARTESIAN_POINT ( 'NONE',  ( -29.36874999999999858, 30.56064500000000095, -3.968750000000000000 ) ) ;
#11293 = CARTESIAN_POINT ( 'NONE',  ( 8.965882632090805160, 11.49625537507852080, 5.536508760620900027 ) ) ;
#11294 = CIRCLE ( 'NONE', #4248, 1.190625000000000488 ) ;
#11295 = CARTESIAN_POINT ( 'NONE',  ( 9.140884278813414809, 13.60098928899521198, -2.935439693214477508 ) ) ;
#11296 = VERTEX_POINT ( 'NONE', #10067 ) ;
#11297 = EDGE_CURVE ( 'NONE', #21613, #16695, #13510, .T. ) ;
#11298 = AXIS2_PLACEMENT_3D ( 'NONE', #6530, #21772, #8180 ) ;
#11299 = CARTESIAN_POINT ( 'NONE',  ( 28.13664483251599790, 1.437813487382768152, 10.63918692494910090 ) ) ;
#11300 = ADVANCED_FACE ( 'NONE', ( #18353 ), #9956, .F. ) ;
#11301 = CARTESIAN_POINT ( 'NONE',  ( 12.26775042526260151, 20.79412849038763156, -1.126120126505927299 ) ) ;
#11302 = EDGE_CURVE ( 'NONE', #5275, #2212, #12677, .T. ) ;
#11303 = CARTESIAN_POINT ( 'NONE',  ( 8.380958430407533299, 20.95884412385370155, 5.503815002083814356 ) ) ;
#11304 = DIRECTION ( 'NONE',  ( -0.9685006480810792739, 0.000000000000000000, -0.2490110332224846346 ) ) ;
#11305 = CARTESIAN_POINT ( 'NONE',  ( 1.864539181856161409, 20.48283743933590273, 4.919364602564411548 ) ) ;
#11306 = DIRECTION ( 'NONE',  ( 0.8606571039906124598, -0.5091849853938075210, 0.000000000000000000 ) ) ;
#11307 = CARTESIAN_POINT ( 'NONE',  ( 30.74535937054756829, 34.52875999999999834, -3.684081112461307317 ) ) ;
#11308 = CARTESIAN_POINT ( 'NONE',  ( 13.60833742269821833, 21.40794255445344163, 2.232467632860299478 ) ) ;
#11309 = VECTOR ( 'NONE', #18488, 1000.000000000000000 ) ;
#11310 = AXIS2_PLACEMENT_3D ( 'NONE', #9568, #13026, #14795 ) ;
#11311 = CARTESIAN_POINT ( 'NONE',  ( 52.65345379380397617, 38.88803500000000213, -16.29354262597895087 ) ) ;
#11312 = CARTESIAN_POINT ( 'NONE',  ( 38.73829298383838449, -5.190444891651378789, -4.197541117638883712 ) ) ;
#11313 = CARTESIAN_POINT ( 'NONE',  ( -0.001888554328890318379, 17.37763432658893947, 0.0008523805038631974973 ) ) ;
#11314 = DIRECTION ( 'NONE',  ( 0.000000000000000000, 1.000000000000000000, 0.000000000000000000 ) ) ;
#11315 = CYLINDRICAL_SURFACE ( 'NONE', #7855, 30.16249999999999076 ) ;
#11316 = CARTESIAN_POINT ( 'NONE',  ( 6.668852574927204735, 11.59258977312087069, 2.757060124530255951 ) ) ;
#11317 = DIRECTION ( 'NONE',  ( 0.000000000000000000, 1.000000000000000000, 0.000000000000000000 ) ) ;
#11318 = CARTESIAN_POINT ( 'NONE',  ( 24.36723594150488026, 39.28205249999999893, 1.799757394719970982 ) ) ;
#11319 = DIRECTION ( 'NONE',  ( -0.9790635044817342925, 0.000000000000000000, 0.2035550397114870846 ) ) ;
#11320 = VECTOR ( 'NONE', #19396, 1000.000000000000000 ) ;
#11321 = ORIENTED_EDGE ( 'NONE', *, *, #9167, .F. ) ;
#11322 = CARTESIAN_POINT ( 'NONE',  ( 44.28293121686854761, -1.983739999999999393, -31.08068102505560759 ) ) ;
#11323 = DIRECTION ( 'NONE',  ( 0.05085730733808393328, 0.000000000000000000, -0.9987059298363656357 ) ) ;
#11324 = ORIENTED_EDGE ( 'NONE', *, *, #15646, .T. ) ;
#11325 = EDGE_CURVE ( 'NONE', #8981, #7494, #21130, .T. ) ;
#11326 = CARTESIAN_POINT ( 'NONE',  ( 11.20042708533316933, 21.25597787441990860, 1.691039092023997492 ) ) ;
#11327 = DIRECTION ( 'NONE',  ( 0.000000000000000000, 1.000000000000000000, 0.000000000000000000 ) ) ;
#11328 = DIRECTION ( 'NONE',  ( 0.9579671649362032637, 0.000000000000000000, -0.2868778675745010664 ) ) ;
#11329 = CARTESIAN_POINT ( 'NONE',  ( 19.37933662139949931, -5.924303267933944461, -14.90337022717902471 ) ) ;
#11330 = CIRCLE ( 'NONE', #7744, 2.381250000000001421 ) ;
#11332 = DIRECTION ( 'NONE',  ( 0.000000000000000000, 1.000000000000000000, 0.000000000000000000 ) ) ;
#11331 = CARTESIAN_POINT ( 'NONE',  ( 0.4158508765940340801, 19.61962022855508181, 7.543245219194639972 ) ) ;
#11333 = ORIENTED_EDGE ( 'NONE', *, *, #11498, .F. ) ;
#11334 =( NAMED_UNIT ( * ) PLANE_ANGLE_UNIT ( ) SI_UNIT ( $, .RADIAN. ) );
#11335 = DIRECTION ( 'NONE',  ( -0.6702301885068628895, 0.000000000000000000, -0.7421532822901579785 ) ) ;
#11336 = DIRECTION ( 'NONE',  ( 0.000000000000000000, -1.000000000000000000, -0.000000000000000000 ) ) ;
#11337 = ORIENTED_EDGE ( 'NONE', *, *, #17995, .F. ) ;
#11338 = CARTESIAN_POINT ( 'NONE',  ( 20.13639834117197935, -1.248927570271565646, -14.78218852182811993 ) ) ;
#11339 = CIRCLE ( 'NONE', #14896, 25.00312500000000426 ) ;
#11340 = CARTESIAN_POINT ( 'NONE',  ( 19.33254070244220557, -0.1605694297987687869, -14.91550252399787091 ) ) ;
#11341 = ORIENTED_EDGE ( 'NONE', *, *, #7933, .F. ) ;
#11342 = CARTESIAN_POINT ( 'NONE',  ( 11.58160216568870737, 11.69841282151974227, -0.9529902506022120967 ) ) ;
#11343 = AXIS2_PLACEMENT_3D ( 'NONE', #3068, #17990, #2846 ) ;
#11344 = CARTESIAN_POINT ( 'NONE',  ( 1.952969610814715207, 9.129395000000000593, 6.747510000000000119 ) ) ;
#11345 = CARTESIAN_POINT ( 'NONE',  ( 9.957248104110922426, 20.90214019755116226, -1.675082132773985322 ) ) ;
#11346 = CARTESIAN_POINT ( 'NONE',  ( -5.863861779363051419, 34.12394749999999988, -34.80955303575778714 ) ) ;
#11347 = DIRECTION ( 'NONE',  ( 0.000000000000000000, 1.000000000000000000, 0.000000000000000000 ) ) ;
#11348 = ORIENTED_EDGE ( 'NONE', *, *, #4417, .T. ) ;
#11349 = CYLINDRICAL_SURFACE ( 'NONE', #8940, 0.7950200000000003930 ) ;
#11350 = DIRECTION ( 'NONE',  ( 0.8624408385128676802, 0.5061578805720818863, 0.000000000000000000 ) ) ;
#11351 = VECTOR ( 'NONE', #12873, 1000.000000000000114 ) ;
#11352 = ORIENTED_EDGE ( 'NONE', *, *, #20441, .F. ) ;
#11353 = ORIENTED_EDGE ( 'NONE', *, *, #6025, .T. ) ;
#11354 = EDGE_CURVE ( 'NONE', #13139, #15569, #13083, .T. ) ;
#11355 = AXIS2_PLACEMENT_3D ( 'NONE', #1447, #1660, #6866 ) ;
#11356 = CARTESIAN_POINT ( 'NONE',  ( 11.33405156777011236, 0.1799087130929279132, -16.79951585329149921 ) ) ;
#11358 = DIRECTION ( 'NONE',  ( -0.2868778675745011220, 0.000000000000000000, -0.9579671649362033747 ) ) ;
#11357 = CARTESIAN_POINT ( 'NONE',  ( 7.186428980350254569, 18.51696245222963455, 8.092093519166050797 ) ) ;
#11359 = EDGE_LOOP ( 'NONE', ( #16656, #19966, #3418, #5445 ) ) ;
#11360 = CARTESIAN_POINT ( 'NONE',  ( 3.724362862741987357, 12.69003629999320282, 0.02154335185942457889 ) ) ;
#11361 = EDGE_LOOP ( 'NONE', ( #12515, #15563, #17433, #16246 ) ) ;
#11362 = AXIS2_PLACEMENT_3D ( 'NONE', #3216, #6538, #10276 ) ;
#11363 = EDGE_LOOP ( 'NONE', ( #658, #3751, #6857, #8610 ) ) ;
#11364 = ADVANCED_FACE ( 'NONE', ( #3011 ), #4778, .F. ) ;
#11365 = ORIENTED_EDGE ( 'NONE', *, *, #6053, .F. ) ;
#11366 = CARTESIAN_POINT ( 'NONE',  ( 2.657223057284000767, 12.04510335958863720, 4.259266508287976372 ) ) ;
#11367 = B_SPLINE_CURVE_WITH_KNOTS ( 'NONE', 3,
 ( #20808, #5677, #2135, #8760 ),
 .UNSPECIFIED., .F., .F.,
 ( 4, 4 ),
 ( -7.968845587666753810E-05, 0.0007517777332624285547 ),
 .UNSPECIFIED. ) ;
#11368 = AXIS2_PLACEMENT_3D ( 'NONE', #3978, #10721, #5743 ) ;
#11369 = AXIS2_PLACEMENT_3D ( 'NONE', #19148, #909, #4014 ) ;
#11370 = VECTOR ( 'NONE', #13707, 1000.000000000000000 ) ;
#11371 = FACE_OUTER_BOUND ( 'NONE', #2778, .T. ) ;
#11372 = CARTESIAN_POINT ( 'NONE',  ( 30.78626241496060700, 9.120187499999998337, -2.552201779827368622 ) ) ;
#11373 = DIRECTION ( 'NONE',  ( 0.2490110332224850509, 0.000000000000000000, -0.9685006480810792739 ) ) ;
#11374 = DIRECTION ( 'NONE',  ( 0.000000000000000000, 1.000000000000000000, 0.000000000000000000 ) ) ;
#11375 = CARTESIAN_POINT ( 'NONE',  ( 3.642152772319685372, 15.74777456311460888, 9.171823029728713550 ) ) ;
#11376 = AXIS2_PLACEMENT_3D ( 'NONE', #2812, #11536, #7785 ) ;
#11377 = VECTOR ( 'NONE', #5095, 1000.000000000000227 ) ;
#11378 = VERTEX_POINT ( 'NONE', #9835 ) ;
#11379 = CARTESIAN_POINT ( 'NONE',  ( -39.34028892251012621, 33.32892749999999893, -14.58007324542170480 ) ) ;
#11380 = CARTESIAN_POINT ( 'NONE',  ( 11.97174136233939556, 21.25996874134203551, -17.62449286037261942 ) ) ;
#11381 = CARTESIAN_POINT ( 'NONE',  ( 13.36585934105912976, 21.37707621349031228, 1.842755075219712380 ) ) ;
#11382 = CARTESIAN_POINT ( 'NONE',  ( 66.03921914090641110, 30.56064500000000095, -11.33033647675950029 ) ) ;
#11383 = VERTEX_POINT ( 'NONE', #16606 ) ;
#11384 = ORIENTED_EDGE ( 'NONE', *, *, #10240, .T. ) ;
#11385 = EDGE_CURVE ( 'NONE', #20069, #6991, #11239, .T. ) ;
#11386 = CARTESIAN_POINT ( 'NONE',  ( 6.092259989090710093, 20.11689778289562014, 0.2466081011508972631 ) ) ;
#11387 = ADVANCED_FACE ( 'NONE', ( #11944 ), #112, .F. ) ;
#11388 = CARTESIAN_POINT ( 'NONE',  ( 10.97968894901760528, 16.77770024244917835, -4.337930532459063571 ) ) ;
#11389 = ORIENTED_EDGE ( 'NONE', *, *, #17622, .T. ) ;
#11390 = VECTOR ( 'NONE', #10579, 1000.000000000000000 ) ;
#11391 = VERTEX_POINT ( 'NONE', #8622 ) ;
#11392 = CYLINDRICAL_SURFACE ( 'NONE', #12388, 0.3962400000000008138 ) ;
#11393 = CARTESIAN_POINT ( 'NONE',  ( 9.192923877405071664, 13.65536061100259069, 6.430361030589125448 ) ) ;
#11394 = CARTESIAN_POINT ( 'NONE',  ( 6.685429349468995142, 11.82209191741327636, 4.133463687248298157 ) ) ;
#11395 = VECTOR ( 'NONE', #139, 1000.000000000000000 ) ;
#11396 = VECTOR ( 'NONE', #20968, 1000.000000000000114 ) ;
#11397 = ADVANCED_FACE ( 'NONE', ( #3769 ), #8835, .T. ) ;
#11398 = AXIS2_PLACEMENT_3D ( 'NONE', #681, #17499, #10641 ) ;
#11399 = CARTESIAN_POINT ( 'NONE',  ( 67.79270099634359781, 30.56064500000000095, -13.76558698117381851 ) ) ;
#11400 = DIRECTION ( 'NONE',  ( 1.000000000000000000, 0.000000000000000000, 0.000000000000000000 ) ) ;
#11401 = CARTESIAN_POINT ( 'NONE',  ( 3.527643555736371450, 13.65542567351872272, -0.8065990906974750407 ) ) ;
#11402 = CARTESIAN_POINT ( 'NONE',  ( 0.3865264268659200919, 11.71693424989172172, 3.209193188785584905 ) ) ;
#11403 = CARTESIAN_POINT ( 'NONE',  ( 1.952969610814715207, 23.41816500000000190, 6.747510000000000119 ) ) ;
#11404 = VERTEX_POINT ( 'NONE', #19003 ) ;
#11405 = CARTESIAN_POINT ( 'NONE',  ( 3.738939841724334467, 14.05232170482083198, -0.1333566731639757863 ) ) ;
#11406 = CARTESIAN_POINT ( 'NONE',  ( 46.03750000000000142, 0.000000000000000000, -10.31874999999999964 ) ) ;
#11407 = CARTESIAN_POINT ( 'NONE',  ( 53.89155349598119926, -5.957381036604508573, -15.70768225484734160 ) ) ;
#11408 = CARTESIAN_POINT ( 'NONE',  ( 16.85565294364209876, -8.302906301136502520, -14.67196852948350561 ) ) ;
#11409 = ORIENTED_EDGE ( 'NONE', *, *, #20038, .T. ) ;
#11410 = DIRECTION ( 'NONE',  ( 0.000000000000000000, 1.000000000000000000, 0.000000000000000000 ) ) ;
#11411 = CARTESIAN_POINT ( 'NONE',  ( 6.174367295332582550, 20.69792818844234361, -0.2343385128640179116 ) ) ;
#11412 = VECTOR ( 'NONE', #11964, 1000.000000000000000 ) ;
#11413 = EDGE_CURVE ( 'NONE', #17451, #16351, #1761, .T. ) ;
#11414 = DIRECTION ( 'NONE',  ( 0.000000000000000000, 1.000000000000000000, 0.000000000000000000 ) ) ;
#11415 = B_SPLINE_CURVE_WITH_KNOTS ( 'NONE', 3,
 ( #29, #8005, #21486, #14777, #1363, #15101, #11651, #6342, #18189, #19829 ),
 .UNSPECIFIED., .F., .F.,
 ( 4, 2, 2, 2, 4 ),
 ( 0.006199817995075669261, 0.006675562902873981644, 0.007151307810672294894, 0.007627052718470608145, 0.008102797626268920528 ),
 .UNSPECIFIED. ) ;
#11416 = CARTESIAN_POINT ( 'NONE',  ( 9.084851576897378322, 16.05738436158114979, -3.614958053632072232 ) ) ;
#11417 = ORIENTED_EDGE ( 'NONE', *, *, #19561, .T. ) ;
#11418 = CARTESIAN_POINT ( 'NONE',  ( 8.826715567800096807, 19.94865183135063091, 6.668355704914617377 ) ) ;
#11419 = DIRECTION ( 'NONE',  ( -0.06191955310929833645, 0.000000000000000000, 0.9980811434661738257 ) ) ;
#11420 = CARTESIAN_POINT ( 'NONE',  ( 0.4722054179714940680, 12.38306287928572047, 3.426248810200787531 ) ) ;
#11421 = DIRECTION ( 'NONE',  ( 0.000000000000000000, 0.000000000000000000, 1.000000000000000000 ) ) ;
#11422 = AXIS2_PLACEMENT_3D ( 'NONE', #12630, #2113, #17496 ) ;
#11423 = EDGE_CURVE ( 'NONE', #4193, #18443, #21142, .T. ) ;
#11424 = CARTESIAN_POINT ( 'NONE',  ( 29.98909767165928386, -5.959792500000001603, -5.214162619065493054 ) ) ;
#11425 = CIRCLE ( 'NONE', #13925, 0.7950199999999982836 ) ;
#11426 = CARTESIAN_POINT ( 'NONE',  ( 13.20757484442835406, 18.50160361240584095, 6.057113864572380102 ) ) ;
#11427 = ADVANCED_FACE ( 'NONE', ( #1094 ), #19559, .F. ) ;
#11428 = DIRECTION ( 'NONE',  ( 0.000000000000000000, 1.000000000000000000, 0.000000000000000000 ) ) ;
#11429 = CARTESIAN_POINT ( 'NONE',  ( 7.417648194976016462, 11.73277151300288246, 5.873043469613717704 ) ) ;
#11430 = EDGE_CURVE ( 'NONE', #21357, #17007, #13751, .T. ) ;
#11431 = CARTESIAN_POINT ( 'NONE',  ( 32.42378190387104553, 34.52875999999999834, -18.15178106273469183 ) ) ;
#11432 = ADVANCED_FACE ( 'NONE', ( #19232 ), #16152, .F. ) ;
#11433 = CARTESIAN_POINT ( 'NONE',  ( 30.41963056417667488, -1.983739999999999837, -8.653862521447852174 ) ) ;
#11434 = CARTESIAN_POINT ( 'NONE',  ( 6.609959801914604860, 11.00164467546537317, 2.731537079386237021 ) ) ;
#11435 = CARTESIAN_POINT ( 'NONE',  ( 29.64606458365116737, 30.55334249999999940, -15.53894806404596096 ) ) ;
#11436 = CARTESIAN_POINT ( 'NONE',  ( 19.93266995306398925, -6.610076642783412559, -15.23350694284797235 ) ) ;
#11437 = CIRCLE ( 'NONE', #1889, 30.16249999999998721 ) ;
#11438 = CARTESIAN_POINT ( 'NONE',  ( -17.46249999999999858, 16.27314499999999953, 10.71562499999999929 ) ) ;
#11439 = ORIENTED_EDGE ( 'NONE', *, *, #7960, .F. ) ;
#11440 = CARTESIAN_POINT ( 'NONE',  ( 55.81697695389291169, -1.983739999999999393, -11.14520323105768362 ) ) ;
#11441 = FACE_OUTER_BOUND ( 'NONE', #9007, .T. ) ;
#11442 = EDGE_LOOP ( 'NONE', ( #657, #18543, #20759, #6246, #7016 ) ) ;
#11443 = CARTESIAN_POINT ( 'NONE',  ( 11.14641082499276337, 21.24872442236535264, 1.545007152345080792 ) ) ;
#11444 = CARTESIAN_POINT ( 'NONE',  ( 29.19635173153840313, 0.000000000000000000, -6.218966092919240296 ) ) ;
#11445 = CARTESIAN_POINT ( 'NONE',  ( 17.20909397020470166, -7.334998182188638083, -15.85734429837840764 ) ) ;
#11447 = CARTESIAN_POINT ( 'NONE',  ( 52.44708915697334106, 0.000000000000000000, 4.020247972991190188 ) ) ;
#11446 = CARTESIAN_POINT ( 'NONE',  ( 1.224586904570614365, 15.68905071955487962, 9.060239213458530116 ) ) ;
#11448 = ORIENTED_EDGE ( 'NONE', *, *, #10097, .F. ) ;
#11449 = DIRECTION ( 'NONE',  ( 0.000000000000000000, 0.000000000000000000, 1.000000000000000000 ) ) ;
#11450 = CARTESIAN_POINT ( 'NONE',  ( 46.03750000000000142, 30.56064500000000095, -10.31874999999999964 ) ) ;
#11451 = VERTEX_POINT ( 'NONE', #17580 ) ;
#11452 = LINE ( 'NONE', #11881, #6859 ) ;
#11453 = AXIS2_PLACEMENT_3D ( 'NONE', #19976, #15550, #18323 ) ;
#11454 = PRODUCT_DEFINITION_SHAPE ( 'NONE', 'NONE',  #1012 ) ;
#11455 = ORIENTED_EDGE ( 'NONE', *, *, #2288, .T. ) ;
#11456 = CARTESIAN_POINT ( 'NONE',  ( 9.535371066084531222, 12.37377145998696193, -1.078836062975678578 ) ) ;
#11457 = ADVANCED_FACE ( 'NONE', ( #7837 ), #21321, .T. ) ;
#11458 = DIRECTION ( 'NONE',  ( 0.9564948366894089338, -0.05542109139015086172, -0.2864369564417716951 ) ) ;
#11459 = ADVANCED_FACE ( 'NONE', ( #10732 ), #2320, .T. ) ;
#11460 = CARTESIAN_POINT ( 'NONE',  ( 11.29892349159651133, 17.71700346048863395, 7.539582004218902789 ) ) ;
#11461 = AXIS2_PLACEMENT_3D ( 'NONE', #9534, #6217, #4788 ) ;
#11462 = CARTESIAN_POINT ( 'NONE',  ( 2.063750000000000195, 30.56064500000000095, -19.71675000000000111 ) ) ;
#11463 = ORIENTED_EDGE ( 'NONE', *, *, #8438, .F. ) ;
#11464 = CARTESIAN_POINT ( 'NONE',  ( 6.906198364295903502, 21.59098349863498001, 1.388813212125012964 ) ) ;
#11465 = CARTESIAN_POINT ( 'NONE',  ( 38.28489021960990613, 38.88803500000000213, 2.732679409805250703 ) ) ;
#11466 = AXIS2_PLACEMENT_3D ( 'NONE', #10824, #19110, #3981 ) ;
#11467 = ORIENTED_EDGE ( 'NONE', *, *, #4044, .F. ) ;
#11468 = ORIENTED_EDGE ( 'NONE', *, *, #5084, .F. ) ;
#11469 = DIRECTION ( 'NONE',  ( -0.9822019212503902974, 0.000000000000000000, 0.1878280753562734662 ) ) ;
#11471 = CARTESIAN_POINT ( 'NONE',  ( 53.08681243026497043, 37.69777154208443193, -16.72443647847455850 ) ) ;
#11470 = CARTESIAN_POINT ( 'NONE',  ( 2.375739369545591284, 11.20929286741210085, 3.469357574953835677 ) ) ;
#11472 = ORIENTED_EDGE ( 'NONE', *, *, #14413, .T. ) ;
#11473 = CARTESIAN_POINT ( 'NONE',  ( 4.920739062717439438, 21.24493168367124341, 1.822501541549086612 ) ) ;
#11474 = EDGE_LOOP ( 'NONE', ( #15324, #14012 ) ) ;
#11475 = ORIENTED_EDGE ( 'NONE', *, *, #20311, .F. ) ;
#11476 = DIRECTION ( 'NONE',  ( -0.2868778675745010664, 0.000000000000000000, -0.9579671649362032637 ) ) ;
#11477 = ORIENTED_EDGE ( 'NONE', *, *, #10902, .F. ) ;
#11478 = AXIS2_PLACEMENT_3D ( 'NONE', #4518, #12832, #16254 ) ;
#11479 = EDGE_CURVE ( 'NONE', #2212, #5275, #2076, .T. ) ;
#11480 = DIRECTION ( 'NONE',  ( 0.000000000000000000, 1.000000000000000000, 0.000000000000000000 ) ) ;
#11481 = CARTESIAN_POINT ( 'NONE',  ( 53.12465760132659653, -7.547403978437176697, -16.68255909309962348 ) ) ;
#11482 = DIRECTION ( 'NONE',  ( 0.000000000000000000, -1.000000000000000000, 0.000000000000000000 ) ) ;
#11483 = CARTESIAN_POINT ( 'NONE',  ( 1.916346363066841585, 18.21153642991714960, -0.3663088864718270221 ) ) ;
#11484 = EDGE_LOOP ( 'NONE', ( #12482, #6339, #7608, #4316 ) ) ;
#11485 = DIRECTION ( 'NONE',  ( 0.000000000000000000, 1.000000000000000000, 0.000000000000000000 ) ) ;
#11486 = PLANE ( 'NONE',  #13875 ) ;
#11487 = CARTESIAN_POINT ( 'NONE',  ( -29.36874999999999858, 2.380615000000000148, 8.731249999999999289 ) ) ;
#11488 = DIRECTION ( 'NONE',  ( 0.000000000000000000, -1.000000000000000000, 0.000000000000000000 ) ) ;
#11489 = VERTEX_POINT ( 'NONE', #17809 ) ;
#11490 = ORIENTED_EDGE ( 'NONE', *, *, #21118, .F. ) ;
#11491 = CARTESIAN_POINT ( 'NONE',  ( 9.014641633456207614, 13.68826078499848187, -2.225326884858752408 ) ) ;
#11492 = DIRECTION ( 'NONE',  ( 0.000000000000000000, 1.000000000000000000, 0.000000000000000000 ) ) ;
#11493 = ORIENTED_EDGE ( 'NONE', *, *, #2745, .T. ) ;
#11494 = AXIS2_PLACEMENT_3D ( 'NONE', #20507, #21152, #9541 ) ;
#11495 = ORIENTED_EDGE ( 'NONE', *, *, #16678, .F. ) ;
#11496 = CARTESIAN_POINT ( 'NONE',  ( -17.46249999999999858, 0.000000000000000000, 0.000000000000000000 ) ) ;
#11497 = CARTESIAN_POINT ( 'NONE',  ( 8.137292697265277042, 11.64158411620971201, 1.582907052082125343 ) ) ;
#11498 = EDGE_CURVE ( 'NONE', #19531, #7380, #15830, .T. ) ;
#11499 = CARTESIAN_POINT ( 'NONE',  ( 2.915917464538113180, -3.968114999999999615, -18.72348548116188027 ) ) ;
#11500 = LINE ( 'NONE', #13185, #7939 ) ;
#11501 = CARTESIAN_POINT ( 'NONE',  ( 0.07126017807656831460, 18.21124384202859048, 0.3721193727441556298 ) ) ;
#11502 = FACE_OUTER_BOUND ( 'NONE', #9135, .T. ) ;
#11503 = VERTEX_POINT ( 'NONE', #18442 ) ;
#11504 = CARTESIAN_POINT ( 'NONE',  ( 7.332923656907011534, 14.94905092387569745, 7.528091012762189393 ) ) ;
#11505 = CARTESIAN_POINT ( 'NONE',  ( 1.532169971477637782, 34.03012968715594866, -20.71839214105750315 ) ) ;
#11506 = CARTESIAN_POINT ( 'NONE',  ( -13.87747867115857936, 36.51313500000000545, -9.458632424640695646 ) ) ;
#11507 = CARTESIAN_POINT ( 'NONE',  ( 17.58883026422746454, -8.071787399390844442, -14.51212895374598055 ) ) ;
#11508 = CARTESIAN_POINT ( 'NONE',  ( -51.02421882195815783, -8.889364999999999739, -23.02637480153789795 ) ) ;
#11509 = ORIENTED_EDGE ( 'NONE', *, *, #14253, .F. ) ;
#11510 = CARTESIAN_POINT ( 'NONE',  ( 11.22752914188877504, 17.71807980195418608, 7.565294845482125830 ) ) ;
#11511 = FACE_OUTER_BOUND ( 'NONE', #2892, .T. ) ;
#11512 = CARTESIAN_POINT ( 'NONE',  ( 10.02357155247649168, 20.86356153117090173, -1.536494726392103383 ) ) ;
#11513 = ORIENTED_EDGE ( 'NONE', *, *, #4721, .F. ) ;
#11514 = CARTESIAN_POINT ( 'NONE',  ( 8.766965087934416090, 20.11665486425001603, 6.515999777456958242 ) ) ;
#11515 = DIRECTION ( 'NONE',  ( 0.000000000000000000, 1.000000000000000000, 0.000000000000000000 ) ) ;
#11516 = CARTESIAN_POINT ( 'NONE',  ( 0.7167346981205086065, 19.54923001721996201, 7.399086397029480011 ) ) ;
#11517 = EDGE_CURVE ( 'NONE', #17560, #16242, #16793, .T. ) ;
#11518 = DIRECTION ( 'NONE',  ( -0.9685006480810794960, 0.000000000000000000, -0.2490110332224836354 ) ) ;
#11519 = CARTESIAN_POINT ( 'NONE',  ( 6.191040577287384217, 20.33851390902405143, 5.218217981261350502 ) ) ;
#11520 = LINE ( 'NONE', #16511, #10397 ) ;
#11521 = VERTEX_POINT ( 'NONE', #15044 ) ;
#11522 = EDGE_CURVE ( 'NONE', #1449, #7354, #14825, .T. ) ;
#11523 = DIRECTION ( 'NONE',  ( 0.000000000000000000, -1.000000000000000000, -0.000000000000000000 ) ) ;
#11524 = EDGE_CURVE ( 'NONE', #11569, #19334, #9926, .T. ) ;
#11525 = CARTESIAN_POINT ( 'NONE',  ( 10.17692691125095905, 21.44638057025442279, 3.378588906132224956 ) ) ;
#11526 = EDGE_CURVE ( 'NONE', #18861, #7013, #7018, .T. ) ;
#11527 = CARTESIAN_POINT ( 'NONE',  ( 38.20361178072028707, -6.037825279267901024, -4.900284418530829633 ) ) ;
#11528 = CARTESIAN_POINT ( 'NONE',  ( 3.722652848722313834, 16.52290265193734342, 9.281875825074834552 ) ) ;
#11529 = FACE_OUTER_BOUND ( 'NONE', #4383, .T. ) ;
#11530 = FACE_OUTER_BOUND ( 'NONE', #21077, .T. ) ;
#11531 = CARTESIAN_POINT ( 'NONE',  ( 42.35466991749225940, -9.531985000000000596, -17.94967221382040279 ) ) ;
#11532 = CARTESIAN_POINT ( 'NONE',  ( 52.80384623828088309, 40.07865999999999929, -16.43108335029171130 ) ) ;
#11533 = FACE_OUTER_BOUND ( 'NONE', #11034, .T. ) ;
#11534 = DIRECTION ( 'NONE',  ( 0.9790635044817341814, 0.000000000000000000, -0.2035550397114870014 ) ) ;
#11535 = ORIENTED_EDGE ( 'NONE', *, *, #15294, .T. ) ;
#11536 = DIRECTION ( 'NONE',  ( -0.3482992169606098920, 0.9330960544336215357, -0.08955115110948595747 ) ) ;
#11537 = CARTESIAN_POINT ( 'NONE',  ( 11.03331691027467620, 12.88648500492797844, 5.466329197351654123 ) ) ;
#11538 = CARTESIAN_POINT ( 'NONE',  ( 21.58408671149279812, -3.402206684524639702, -14.97329867675111537 ) ) ;
#11539 = CARTESIAN_POINT ( 'NONE',  ( 55.33978576324753362, 34.52875999999999834, -23.05096232720518756 ) ) ;
#11540 = ORIENTED_EDGE ( 'NONE', *, *, #17190, .T. ) ;
#11541 = CARTESIAN_POINT ( 'NONE',  ( 12.80846360209676682, 12.10654534839631147, 4.257358460916016440 ) ) ;
#11542 = FACE_BOUND ( 'NONE', #15430, .T. ) ;
#11543 = VECTOR ( 'NONE', #21270, 1000.000000000000000 ) ;
#11544 = CARTESIAN_POINT ( 'NONE',  ( 6.160630842786900097, 11.06731641207071171, 1.862947408479730615 ) ) ;
#11545 = CARTESIAN_POINT ( 'NONE',  ( 19.94507429925241127, -1.548276246954950697, -14.95858684565857644 ) ) ;
#11547 = DIRECTION ( 'NONE',  ( 0.6496772031432432870, 0.000000000000000000, -0.7602101891687411683 ) ) ;
#11546 = CARTESIAN_POINT ( 'NONE',  ( -0.1868151138448943538, 17.21628798890151302, 0.7963446044912158017 ) ) ;
#11548 = ORIENTED_EDGE ( 'NONE', *, *, #7340, .F. ) ;
#11549 = ADVANCED_FACE ( 'NONE', ( #21428 ), #9839, .T. ) ;
#11550 = FACE_OUTER_BOUND ( 'NONE', #12878, .T. ) ;
#11551 = PRODUCT_DEFINITION ( 'UNKNOWN', '', #17246, #826 ) ;
#11552 = ORIENTED_EDGE ( 'NONE', *, *, #1009, .F. ) ;
#11553 = CARTESIAN_POINT ( 'NONE',  ( 2.417820406479087580, -0.9589899600121986056, -22.53959718991430350 ) ) ;
#11554 = ADVANCED_FACE ( 'NONE', ( #9602 ), #10044, .T. ) ;
#11555 = EDGE_LOOP ( 'NONE', ( #10045, #16743, #21322, #933 ) ) ;
#11556 = CARTESIAN_POINT ( 'NONE',  ( 8.501533767468714586, 20.63193666139594029, 0.2033124972060851021 ) ) ;
#11557 = EDGE_CURVE ( 'NONE', #5914, #19210, #6676, .T. ) ;
#11558 = CARTESIAN_POINT ( 'NONE',  ( 2.275221076386582997, 18.57027319413175803, 0.6409314954482938642 ) ) ;
#11559 = DIRECTION ( 'NONE',  ( -0.2868778675745011220, 0.000000000000000000, -0.9579671649362034858 ) ) ;
#11560 = CARTESIAN_POINT ( 'NONE',  ( 9.207550040625500642, 18.56570064461385527, 7.657528539673981172 ) ) ;
#11561 = AXIS2_PLACEMENT_3D ( 'NONE', #17111, #12355, #15574 ) ;
#11562 = CARTESIAN_POINT ( 'NONE',  ( 14.99032816781414290, -7.116660944607684058, -16.28946189193466054 ) ) ;
#11563 = DIRECTION ( 'NONE',  ( -0.000000000000000000, -1.000000000000000000, 0.000000000000000000 ) ) ;
#11564 = VERTEX_POINT ( 'NONE', #2869 ) ;
#11565 = CARTESIAN_POINT ( 'NONE',  ( 10.44409366562669383, 19.92218912599375003, 5.282434299519857213 ) ) ;
#11566 = CARTESIAN_POINT ( 'NONE',  ( 9.061749118141319670, 15.28249587578532065, -3.643789211875564149 ) ) ;
#11567 = DIRECTION ( 'NONE',  ( 0.05085730733808393328, 0.000000000000000000, -0.9987059298363656357 ) ) ;
#11568 = EDGE_LOOP ( 'NONE', ( #15288, #841, #19740, #13684 ) ) ;
#11569 = VERTEX_POINT ( 'NONE', #13056 ) ;
#11570 = CARTESIAN_POINT ( 'NONE',  ( 54.11611804786240043, 1.984375000000000000, -30.58983753981140197 ) ) ;
#11572 = DIRECTION ( 'NONE',  ( -0.6702301885068632226, 0.000000000000000000, -0.7421532822901577564 ) ) ;
#11571 = CARTESIAN_POINT ( 'NONE',  ( 2.722583763829597547, 20.92902966678202148, 1.865821207828856743 ) ) ;
#11573 = EDGE_LOOP ( 'NONE', ( #13469, #8906, #14471, #18882, #10733, #178, #2971, #19744, #385, #256, #5830, #1532, #8992, #10714, #13195, #5891, #15131, #21649, #6785, #18316, #3177 ) ) ;
#11574 = CARTESIAN_POINT ( 'NONE',  ( 7.495216218794918284, 16.57436198711859632, 8.387193370074408350 ) ) ;
#11575 = ADVANCED_FACE ( 'NONE', ( #6516 ), #1631, .T. ) ;
#11576 = ORIENTED_EDGE ( 'NONE', *, *, #1670, .F. ) ;
#11577 = ADVANCED_FACE ( 'NONE', ( #11595 ), #21536, .T. ) ;
#11578 = EDGE_CURVE ( 'NONE', #19311, #19208, #21491, .T. ) ;
#11579 = VECTOR ( 'NONE', #2428, 1000.000000000000000 ) ;
#11580 = ORIENTED_EDGE ( 'NONE', *, *, #21663, .F. ) ;
#11581 = DIRECTION ( 'NONE',  ( 0.000000000000000000, -1.000000000000000000, 0.000000000000000000 ) ) ;
#11582 = ORIENTED_EDGE ( 'NONE', *, *, #8951, .F. ) ;
#11583 = CARTESIAN_POINT ( 'NONE',  ( 2.181769368323757785, 12.69882926080645547, 2.054496759014617702 ) ) ;
#11584 = CARTESIAN_POINT ( 'NONE',  ( 10.92073974459310115, 21.80709644552430149, -0.001139687782708651703 ) ) ;
#11585 = CARTESIAN_POINT ( 'NONE',  ( 3.965678348075499127, 12.88004042469166244, 0.9588226284739858052 ) ) ;
#11586 = DIRECTION ( 'NONE',  ( 0.3697464814795229371, -0.9291326812858928808, 0.000000000000000000 ) ) ;
#11587 = FACE_OUTER_BOUND ( 'NONE', #20533, .T. ) ;
#11588 = CARTESIAN_POINT ( 'NONE',  ( 49.72033008250774344, 42.06303499999999929, -2.687827786179598277 ) ) ;
#11589 = CARTESIAN_POINT ( 'NONE',  ( 2.287589871148618226, 19.69045419824025345, 0.4926734596364841234 ) ) ;
#11590 = VECTOR ( 'NONE', #20498, 1000.000000000000114 ) ;
#11591 = ORIENTED_EDGE ( 'NONE', *, *, #9221, .F. ) ;
#11592 = CARTESIAN_POINT ( 'NONE',  ( 61.56621290189396944, 0.000000000000000000, -0.7977859469341201937 ) ) ;
#11593 = CARTESIAN_POINT ( 'NONE',  ( 36.80301088673436283, 0.000000000000000000, -23.10021947667301134 ) ) ;
#11594 = LINE ( 'NONE', #18008, #10305 ) ;
#11595 = FACE_OUTER_BOUND ( 'NONE', #18957, .T. ) ;
#11596 = VERTEX_POINT ( 'NONE', #18331 ) ;
#11597 = VERTEX_POINT ( 'NONE', #2987 ) ;
#11598 = CARTESIAN_POINT ( 'NONE',  ( 5.651664637997457774, 18.85032048260596227, -0.8301301036730029947 ) ) ;
#11599 = LINE ( 'NONE', #18133, #5889 ) ;
#11600 = VERTEX_POINT ( 'NONE', #9711 ) ;
#11601 = EDGE_LOOP ( 'NONE', ( #5634, #12896, #16675, #19825 ) ) ;
#11602 = EDGE_CURVE ( 'NONE', #21211, #10152, #667, .T. ) ;
#11603 = FACE_OUTER_BOUND ( 'NONE', #20173, .T. ) ;
#11604 = ORIENTED_EDGE ( 'NONE', *, *, #4535, .T. ) ;
#11605 = CARTESIAN_POINT ( 'NONE',  ( 9.224670804798329016, 13.97085982373057789, 6.622973666382621971 ) ) ;
#11606 = CARTESIAN_POINT ( 'NONE',  ( 7.017598957091650824, 12.50116773309939155, 5.654779006795910057 ) ) ;
#11607 = CIRCLE ( 'NONE', #1349, 0.3962400000000008138 ) ;
#11608 = DIRECTION ( 'NONE',  ( 0.8583349619704310207, 0.000000000000000000, -0.5130897514657826175 ) ) ;
#11609 = CARTESIAN_POINT ( 'NONE',  ( 31.68988926855799448, 34.52875999999999834, 1.626235259850384418 ) ) ;
#11610 = DIRECTION ( 'NONE',  ( 0.000000000000000000, 1.000000000000000000, 0.000000000000000000 ) ) ;
#11611 = CARTESIAN_POINT ( 'NONE',  ( 2.254006964870530982, 19.81104553907935895, 0.4638622323098755551 ) ) ;
#11612 = CARTESIAN_POINT ( 'NONE',  ( -0.1927777004839320296, 15.08680665703588097, 0.2075260073429413266 ) ) ;
#11613 = LINE ( 'NONE', #9950, #346 ) ;
#11614 = EDGE_LOOP ( 'NONE', ( #2162, #16094, #21041, #15204 ) ) ;
#11615 = CARTESIAN_POINT ( 'NONE',  ( 1.095975960959599149, 19.74033803598106118, 2.122738190115129431 ) ) ;
#11616 = DIRECTION ( 'NONE',  ( 0.000000000000000000, -1.000000000000000000, 0.000000000000000000 ) ) ;
#11617 = CARTESIAN_POINT ( 'NONE',  ( 15.23205103213198441, 19.43957250000000059, -19.24493258192747902 ) ) ;
#11618 = DIRECTION ( 'NONE',  ( -0.2672484743474500268, 0.000000000000000000, -0.9636276526537417286 ) ) ;
#11619 = ORIENTED_EDGE ( 'NONE', *, *, #2742, .F. ) ;
#11620 = CARTESIAN_POINT ( 'NONE',  ( 12.38698366852240440, 10.42448595387692301, 2.757262531655723770 ) ) ;
#11621 = AXIS2_PLACEMENT_3D ( 'NONE', #6181, #14385, #14613 ) ;
#11622 = DIRECTION ( 'NONE',  ( 1.000000000000000000, 0.000000000000000000, 0.000000000000000000 ) ) ;
#11623 = CARTESIAN_POINT ( 'NONE',  ( 9.863601304476318887, 20.48082896158547683, -1.957850357342349357 ) ) ;
#11624 = VERTEX_POINT ( 'NONE', #10477 ) ;
#11625 = EDGE_CURVE ( 'NONE', #5229, #16209, #10587, .T. ) ;
#11626 = CARTESIAN_POINT ( 'NONE',  ( 9.187132663661900622, 18.55511614605454795, 7.533150477718545623 ) ) ;
#11627 = DIRECTION ( 'NONE',  ( 0.9685006480810792739, -0.000000000000000000, 0.2490110332224850509 ) ) ;
#11628 = VECTOR ( 'NONE', #4025, 1000.000000000000000 ) ;
#11629 = CARTESIAN_POINT ( 'NONE',  ( 6.302243142281915844, 11.75769050285926198, 2.431337456366345240 ) ) ;
#11630 = CARTESIAN_POINT ( 'NONE',  ( 6.357652142832493247, 20.10075509776510572, 5.647861525684289674 ) ) ;
#11631 = CARTESIAN_POINT ( 'NONE',  ( 29.19635173153840313, 1.984375000000000000, -6.218966092919240296 ) ) ;
#11632 = ORIENTED_EDGE ( 'NONE', *, *, #14653, .T. ) ;
#11633 = CARTESIAN_POINT ( 'NONE',  ( 11.62556940365261759, 17.61531206902142799, 7.032413415529686240 ) ) ;
#11634 = CARTESIAN_POINT ( 'NONE',  ( 1.773193521281420049, 13.91834099111223111, 9.084643052167260535 ) ) ;
#11635 = CARTESIAN_POINT ( 'NONE',  ( 29.45491884992628329, -1.983739999999999393, -15.58809351040512325 ) ) ;
#11636 = CARTESIAN_POINT ( 'NONE',  ( 48.58367710892853353, 0.000000000000000000, -25.32442392637788231 ) ) ;
#11637 = AXIS2_PLACEMENT_3D ( 'NONE', #17209, #73, #5256 ) ;
#11638 = CARTESIAN_POINT ( 'NONE',  ( 52.79771328282338771, 32.54502000000000095, 3.317700572842066986 ) ) ;
#11639 = CARTESIAN_POINT ( 'NONE',  ( 44.27024749654656688, 38.88803500000000213, -8.722764363618033201 ) ) ;
#11640 = DIRECTION ( 'NONE',  ( 0.000000000000000000, 1.000000000000000000, 0.000000000000000000 ) ) ;
#11641 = CARTESIAN_POINT ( 'NONE',  ( 19.99312429566830218, -95.96551800000000298, -11.46559883803463720 ) ) ;
#11642 = CIRCLE ( 'NONE', #12706, 0.7950200000000006151 ) ;
#11643 = DIRECTION ( 'NONE',  ( 0.000000000000000000, 1.000000000000000000, 0.000000000000000000 ) ) ;
#11644 = ORIENTED_EDGE ( 'NONE', *, *, #16040, .F. ) ;
#11645 = CARTESIAN_POINT ( 'NONE',  ( 20.76310168089343478, -3.968114999999999615, -11.26763008640078212 ) ) ;
#11646 = ORIENTED_EDGE ( 'NONE', *, *, #20136, .F. ) ;
#11647 = EDGE_CURVE ( 'NONE', #7172, #19536, #15578, .T. ) ;
#11648 = CARTESIAN_POINT ( 'NONE',  ( 12.71963864430030533, 19.02334098581724575, 5.664408184932725021 ) ) ;
#11649 = VECTOR ( 'NONE', #4905, 1000.000000000000000 ) ;
#11650 = CARTESIAN_POINT ( 'NONE',  ( 57.69402548289047417, 32.54502000000000095, -20.84562559047711261 ) ) ;
#11651 = CARTESIAN_POINT ( 'NONE',  ( 52.31827865322838278, 38.27710895709835626, -17.47985049647301636 ) ) ;
#11652 = EDGE_CURVE ( 'NONE', #5927, #19979, #8802, .T. ) ;
#11653 = CARTESIAN_POINT ( 'NONE',  ( 12.12836021491582983, -0.4634883892451792109, -16.16564750685157748 ) ) ;
#11654 = DIRECTION ( 'NONE',  ( 0.000000000000000000, -1.000000000000000000, 0.000000000000000000 ) ) ;
#11655 = ORIENTED_EDGE ( 'NONE', *, *, #19326, .T. ) ;
#11656 = CARTESIAN_POINT ( 'NONE',  ( -0.2842592608159666967, 21.03045532464439304, 5.180682183037808031 ) ) ;
#11657 = CARTESIAN_POINT ( 'NONE',  ( 3.885799590448840046, 17.39673999151104056, -0.5543496090295351175 ) ) ;
#11658 = VERTEX_POINT ( 'NONE', #415 ) ;
#11659 = AXIS2_PLACEMENT_3D ( 'NONE', #7862, #6420, #14639 ) ;
#11660 = CARTESIAN_POINT ( 'NONE',  ( 6.081787118896238020, 11.54994109032966065, 2.929746488810360816 ) ) ;
#11661 = AXIS2_PLACEMENT_3D ( 'NONE', #6482, #13449, #3059 ) ;
#11662 = ORIENTED_EDGE ( 'NONE', *, *, #3722, .T. ) ;
#11663 = CARTESIAN_POINT ( 'NONE',  ( 12.22544842876060400, 20.89247853322200044, -1.170216963302677549 ) ) ;
#11664 = CARTESIAN_POINT ( 'NONE',  ( 38.96848998618624904, 40.07865999999999929, -3.934807454472129429 ) ) ;
#11665 = CARTESIAN_POINT ( 'NONE',  ( 11.39060897379513371, 13.68327412096624229, 7.089011163150622075 ) ) ;
#11666 = AXIS2_PLACEMENT_3D ( 'NONE', #18260, #1666, #18364 ) ;
#11667 = EDGE_CURVE ( 'NONE', #10917, #21188, #15258, .T. ) ;
#11668 = CARTESIAN_POINT ( 'NONE',  ( 11.87797320575361049, -2.913634519652867461, -16.82300781167370829 ) ) ;
#11669 = CARTESIAN_POINT ( 'NONE',  ( 14.28908772023590323, 15.36419388438619649, -17.51222415809595390 ) ) ;
#11670 = VERTEX_POINT ( 'NONE', #8479 ) ;
#11671 = VECTOR ( 'NONE', #21185, 1000.000000000000000 ) ;
#11672 = CARTESIAN_POINT ( 'NONE',  ( 9.338416706065666872, 21.08959124998475332, 2.363483124878559938 ) ) ;
#11673 = CARTESIAN_POINT ( 'NONE',  ( 13.29031052474874919, 12.74100552075486270, 6.136694359698553924 ) ) ;
#11674 = CARTESIAN_POINT ( 'NONE',  ( -2.607150795738780058, 32.54502000000000095, 8.731885000000000119 ) ) ;
#11675 = ORIENTED_EDGE ( 'NONE', *, *, #5793, .T. ) ;
#11676 = ORIENTED_EDGE ( 'NONE', *, *, #11578, .F. ) ;
#11677 = DIRECTION ( 'NONE',  ( 0.000000000000000000, 1.000000000000000000, 0.000000000000000000 ) ) ;
#11678 = EDGE_CURVE ( 'NONE', #1714, #11160, #8778, .T. ) ;
#11680 = PLANE ( 'NONE',  #16983 ) ;
#11679 = CARTESIAN_POINT ( 'NONE',  ( 5.268927068550723014, 12.34694125381258267, 7.212504574052345241 ) ) ;
#11681 = B_SPLINE_CURVE_WITH_KNOTS ( 'NONE', 3,
 ( #17216, #17114, #192, #2291 ),
 .UNSPECIFIED., .F., .F.,
 ( 4, 4 ),
 ( 0.000000000000000000, 1.000000000000000000 ),
 .UNSPECIFIED. ) ;
#11682 = ORIENTED_EDGE ( 'NONE', *, *, #10577, .F. ) ;
#11683 = CARTESIAN_POINT ( 'NONE',  ( 6.259225472249761779, 21.09377974628283070, 5.464090393452734951 ) ) ;
#11684 = AXIS2_PLACEMENT_3D ( 'NONE', #5949, #19002, #17578 ) ;
#11685 = EDGE_LOOP ( 'NONE', ( #14250, #20396, #6068, #7156 ) ) ;
#11686 = ORIENTED_EDGE ( 'NONE', *, *, #19187, .T. ) ;
#11687 = CARTESIAN_POINT ( 'NONE',  ( 0.1316005820730320741, 13.64832906318255645, 1.788781926648060239 ) ) ;
#11688 = DIRECTION ( 'NONE',  ( -0.000000000000000000, -1.000000000000000000, 0.000000000000000000 ) ) ;
#11689 = ORIENTED_EDGE ( 'NONE', *, *, #11251, .F. ) ;
#11690 = STYLED_ITEM ( 'NONE', ( #16939 ), #13947 ) ;
#11691 = CARTESIAN_POINT ( 'NONE',  ( 13.14098188209254836, 22.19922814609550343, 0.3112431406973831249 ) ) ;
#11692 = CARTESIAN_POINT ( 'NONE',  ( 4.296840172830673765, 12.04396863174460997, 2.515640464070328708 ) ) ;
#11693 = LINE ( 'NONE', #15468, #19845 ) ;
#11694 = ADVANCED_FACE ( 'NONE', ( #20400 ), #11917, .F. ) ;
#11695 = AXIS2_PLACEMENT_3D ( 'NONE', #920, #19374, #6320 ) ;
#11696 = DIRECTION ( 'NONE',  ( 0.000000000000000000, 0.000000000000000000, 1.000000000000000000 ) ) ;
#11697 = CARTESIAN_POINT ( 'NONE',  ( 1.893982906205322392, 12.64452536331596733, 0.8755402015730822107 ) ) ;
#11698 = EDGE_CURVE ( 'NONE', #1762, #20415, #6721, .T. ) ;
#11699 = EDGE_CURVE ( 'NONE', #7796, #17229, #13933, .T. ) ;
#11700 = AXIS2_PLACEMENT_3D ( 'NONE', #16900, #1748, #15899 ) ;
#11701 = ORIENTED_EDGE ( 'NONE', *, *, #7265, .F. ) ;
#11702 = VECTOR ( 'NONE', #8227, 1000.000000000000000 ) ;
#11703 = CARTESIAN_POINT ( 'NONE',  ( 42.35466991749225940, 42.06303499999999929, -17.94967221382040279 ) ) ;
#11704 = DIRECTION ( 'NONE',  ( 0.9129422336036123742, 0.000000000000000000, -0.4080888115384289083 ) ) ;
#11705 = DIRECTION ( 'NONE',  ( -0.9685006480810791629, 0.000000000000000000, -0.2490110332224850509 ) ) ;
#11706 = CARTESIAN_POINT ( 'NONE',  ( 53.10651001381376091, 40.07865999999999929, -16.70269254552787075 ) ) ;
#11707 = ORIENTED_EDGE ( 'NONE', *, *, #8549, .F. ) ;
#11708 = VERTEX_POINT ( 'NONE', #3412 ) ;
#11709 = VECTOR ( 'NONE', #15500, 1000.000000000000114 ) ;
#11710 = CARTESIAN_POINT ( 'NONE',  ( 13.82296214138276014, 20.66289627653780059, 3.967640175402189051 ) ) ;
#11711 = CARTESIAN_POINT ( 'NONE',  ( 0.8632392633340351118, 20.20131944153736114, 7.855970746976047359 ) ) ;
#11712 = ORIENTED_EDGE ( 'NONE', *, *, #21811, .T. ) ;
#11713 = AXIS2_PLACEMENT_3D ( 'NONE', #7866, #11410, #1235 ) ;
#11714 = ORIENTED_EDGE ( 'NONE', *, *, #20309, .F. ) ;
#11715 = LINE ( 'NONE', #19887, #1433 ) ;
#11716 = ORIENTED_EDGE ( 'NONE', *, *, #7092, .T. ) ;
#11717 = CARTESIAN_POINT ( 'NONE',  ( 9.228806684017154538, 16.38677358761131586, 7.225591685826160848 ) ) ;
#11718 = VECTOR ( 'NONE', #6567, 1000.000000000000000 ) ;
#11719 = AXIS2_PLACEMENT_3D ( 'NONE', #6539, #3217, #9629 ) ;
#11720 = CIRCLE ( 'NONE', #16994, 1.190625000000000488 ) ;
#11721 = CARTESIAN_POINT ( 'NONE',  ( 2.845659021318093007, 19.08034105350286325, 7.444203947204882432 ) ) ;
#11722 = CIRCLE ( 'NONE', #1128, 0.5080000000000013394 ) ;
#11723 = CIRCLE ( 'NONE', #6435, 1.587499999999998579 ) ;
#11724 = DIRECTION ( 'NONE',  ( 0.2490110332224857170, 0.000000000000000000, -0.9685006480810790519 ) ) ;
#11725 = DIRECTION ( 'NONE',  ( -0.8609107660235849613, 0.000000000000000000, 0.5087559856598092844 ) ) ;
#11726 = CARTESIAN_POINT ( 'NONE',  ( -0.1105414598945317628, 13.63446969317437762, 0.8406885842557084709 ) ) ;
#11727 = EDGE_CURVE ( 'NONE', #1050, #15435, #16570, .T. ) ;
#11728 = CARTESIAN_POINT ( 'NONE',  ( 59.10939610998308780, 0.000000000000000000, -2.797471275456639539 ) ) ;
#11729 = ORIENTED_EDGE ( 'NONE', *, *, #2511, .F. ) ;
#11730 = CARTESIAN_POINT ( 'NONE',  ( -0.3546834805565413640, 20.13283946025274318, 3.854164455137035095 ) ) ;
#11731 = DIRECTION ( 'NONE',  ( 1.000000000000000000, 0.000000000000000000, 0.000000000000000000 ) ) ;
#11732 = CARTESIAN_POINT ( 'NONE',  ( 52.27672133479757832, -6.045805788883473753, -17.51606593332607176 ) ) ;
#11733 = CARTESIAN_POINT ( 'NONE',  ( 13.67756757867809725, 12.29391749999999739, 2.571257636385987144 ) ) ;
#11734 = CARTESIAN_POINT ( 'NONE',  ( -46.55710204590916135, 41.43438499999999891, -7.870588902259476605 ) ) ;
#11735 = AXIS2_PLACEMENT_3D ( 'NONE', #4943, #8687, #21751 ) ;
#11736 = ORIENTED_EDGE ( 'NONE', *, *, #18905, .T. ) ;
#11737 = VECTOR ( 'NONE', #6147, 1000.000000000000114 ) ;
#11738 = CARTESIAN_POINT ( 'NONE',  ( 8.857113657072135382, 13.36844392990906272, -2.751357805998382311 ) ) ;
#11739 = CYLINDRICAL_SURFACE ( 'NONE', #7475, 2.381250000000001421 ) ;
#11740 = CARTESIAN_POINT ( 'NONE',  ( 12.04010895967688732, 21.53301061183326226, 4.011024392964848140 ) ) ;
#11741 = ORIENTED_EDGE ( 'NONE', *, *, #10430, .T. ) ;
#11742 = AXIS2_PLACEMENT_3D ( 'NONE', #17430, #17195, #12458 ) ;
#11743 = CARTESIAN_POINT ( 'NONE',  ( 6.923392622719085843, 21.50917362703793145, 1.522476032831644233 ) ) ;
#11744 = AXIS2_PLACEMENT_3D ( 'NONE', #20734, #5589, #12350 ) ;
#11745 = FACE_OUTER_BOUND ( 'NONE', #11363, .T. ) ;
#11746 = CARTESIAN_POINT ( 'NONE',  ( -3.929154139288399961, 23.41816500000000190, 0.9374890779182719625 ) ) ;
#11747 = DIRECTION ( 'NONE',  ( 0.000000000000000000, -1.000000000000000000, 0.000000000000000000 ) ) ;
#11748 = CARTESIAN_POINT ( 'NONE',  ( 6.204561899348269627, 20.32115355487759700, 5.253253164602614156 ) ) ;
#11749 = CARTESIAN_POINT ( 'NONE',  ( 0.7843704457339527591, 34.12394749999999988, -23.55949434567611078 ) ) ;
#11750 = AXIS2_PLACEMENT_3D ( 'NONE', #291, #13369, #4846 ) ;
#11751 = CARTESIAN_POINT ( 'NONE',  ( 10.46803433819026097, 20.58315642183951866, -1.567353574707110120 ) ) ;
#11752 = CARTESIAN_POINT ( 'NONE',  ( 5.367955360089083250, 14.66436098424711787, 7.720591347676860394 ) ) ;
#11753 = CARTESIAN_POINT ( 'NONE',  ( 1.663896921981091070, 13.92038700339129242, 9.113439979769390575 ) ) ;
#11754 = DIRECTION ( 'NONE',  ( 0.000000000000000000, -1.000000000000000000, 0.000000000000000000 ) ) ;
#11755 = EDGE_CURVE ( 'NONE', #20322, #10480, #6313, .T. ) ;
#11756 = AXIS2_PLACEMENT_3D ( 'NONE', #13714, #6849, #12042 ) ;
#11757 = LINE ( 'NONE', #14871, #1496 ) ;
#11758 = CARTESIAN_POINT ( 'NONE',  ( 1.281390429963812361, 20.33449649584820307, 3.528586641614371633 ) ) ;
#11759 = CARTESIAN_POINT ( 'NONE',  ( 55.33978576324753362, 34.52875999999999834, -23.05096232720518756 ) ) ;
#11760 = FACE_OUTER_BOUND ( 'NONE', #12979, .T. ) ;
#11761 = CARTESIAN_POINT ( 'NONE',  ( 14.27942466917048492, -8.136872695340121808, -16.45546583691613662 ) ) ;
#11762 = CARTESIAN_POINT ( 'NONE',  ( 53.84486179190094646, -76.79125307200000350, -6.412645463410259872 ) ) ;
#11763 = EDGE_LOOP ( 'NONE', ( #3959, #15342 ) ) ;
#11764 = CARTESIAN_POINT ( 'NONE',  ( 49.28028498622276032, 34.52875999999999834, -25.68670502218146368 ) ) ;
#11765 = CARTESIAN_POINT ( 'NONE',  ( 10.69728709731364802, 11.77315711255725184, 3.903429647405576297 ) ) ;
#11766 = CARTESIAN_POINT ( 'NONE',  ( 44.27024749654656688, 38.88803500000000213, -8.722764363618033201 ) ) ;
#11767 = AXIS2_PLACEMENT_3D ( 'NONE', #17805, #6064, #11485 ) ;
#11768 = LINE ( 'NONE', #18494, #4996 ) ;
#11769 = CARTESIAN_POINT ( 'NONE',  ( 13.05013046055113257, 13.27867918978523143, 5.430472891953736614 ) ) ;
#11770 = DIRECTION ( 'NONE',  ( -0.9685006480810791629, 0.000000000000000000, -0.2490110332224850509 ) ) ;
#11771 = CARTESIAN_POINT ( 'NONE',  ( 12.31258714455350045, -6.210927838223190278, -15.15504894760450227 ) ) ;
#11773 = CARTESIAN_POINT ( 'NONE',  ( 1.854799496439154316, 13.08893749999999834, 3.211081754263136911 ) ) ;
#11772 = CARTESIAN_POINT ( 'NONE',  ( 1.277855706708208139, 17.15958586172077460, 8.877528151527451783 ) ) ;
#11774 = ORIENTED_EDGE ( 'NONE', *, *, #5973, .F. ) ;
#11775 = CARTESIAN_POINT ( 'NONE',  ( 0.000000000000000000, 0.000000000000000000, 0.000000000000000000 ) ) ;
#11776 = CYLINDRICAL_SURFACE ( 'NONE', #20130, 9.524999999999998579 ) ;
#11777 = CARTESIAN_POINT ( 'NONE',  ( 6.153511036807811863, 11.00164291183192233, 2.868232663458314402 ) ) ;
#11778 = ORIENTED_EDGE ( 'NONE', *, *, #15488, .T. ) ;
#11779 = CARTESIAN_POINT ( 'NONE',  ( 6.387440882495097227, 20.04707047619034199, 0.2130560995154684445 ) ) ;
#11780 = CARTESIAN_POINT ( 'NONE',  ( 11.32770823999889842, 21.35684717879324168, 1.982554180330467153 ) ) ;
#11781 = CARTESIAN_POINT ( 'NONE',  ( 38.86427657468069441, 37.69740999999999786, -4.050204114804302868 ) ) ;
#11782 = CARTESIAN_POINT ( 'NONE',  ( 7.825123033775229331, 20.10277937464278253, -1.660880645940871592 ) ) ;
#11783 = EDGE_CURVE ( 'NONE', #20277, #21616, #13481, .T. ) ;
#11784 = CARTESIAN_POINT ( 'NONE',  ( 14.23877267092113108, -6.845582297732573984, -16.44448175767178100 ) ) ;
#11785 = SURFACE_SIDE_STYLE ('',( #21399 ) ) ;
#11786 = AXIS2_PLACEMENT_3D ( 'NONE', #17203, #3728, #179 ) ;
#11787 = ORIENTED_EDGE ( 'NONE', *, *, #6028, .F. ) ;
#11788 = CARTESIAN_POINT ( 'NONE',  ( 8.542329699723902436, 20.53907793869597853, 0.2423800136953121742 ) ) ;
#11789 = CARTESIAN_POINT ( 'NONE',  ( 11.52456251676331078, 10.98707485392928085, -1.337784965846495089 ) ) ;
#11790 = DIRECTION ( 'NONE',  ( 0.05085730733808393328, 0.000000000000000000, -0.9987059298363656357 ) ) ;
#11791 = ORIENTED_EDGE ( 'NONE', *, *, #1727, .F. ) ;
#11792 = ORIENTED_EDGE ( 'NONE', *, *, #7483, .T. ) ;
#11793 = CARTESIAN_POINT ( 'NONE',  ( 53.14266576735293768, -5.167590446840315543, -16.66242751532468702 ) ) ;
#11794 = CARTESIAN_POINT ( 'NONE',  ( 11.29480541571663110, 19.06662053919708555, -3.732521424140298638 ) ) ;
#11796 = LINE ( 'NONE', #61, #6379 ) ;
#11795 = CARTESIAN_POINT ( 'NONE',  ( -0.02599706384783656565, 20.87305502788824185, 6.462324260655689656 ) ) ;
#11797 = ORIENTED_EDGE ( 'NONE', *, *, #1514, .F. ) ;
#11798 = CARTESIAN_POINT ( 'NONE',  ( 7.379864355900540573, 17.67279214094323692, 8.233010488899299872 ) ) ;
#11799 = VECTOR ( 'NONE', #7965, 1000.000000000000000 ) ;
#11800 = ORIENTED_EDGE ( 'NONE', *, *, #2950, .F. ) ;
#11801 = EDGE_CURVE ( 'NONE', #5219, #4077, #9131, .T. ) ;
#11802 = DIRECTION ( 'NONE',  ( -0.08420877549337300871, 0.000000000000000000, -0.9964481331860212121 ) ) ;
#11803 = VERTEX_POINT ( 'NONE', #3849 ) ;
#11804 = CARTESIAN_POINT ( 'NONE',  ( 1.948622324866731370, 13.89757314177814074, 0.8249782737054650594 ) ) ;
#11805 = AXIS2_PLACEMENT_3D ( 'NONE', #14605, #9703, #11255 ) ;
#11806 = EDGE_CURVE ( 'NONE', #11708, #21099, #17219, .T. ) ;
#11807 = CARTESIAN_POINT ( 'NONE',  ( 3.798072540083225590, 13.90936388833114634, 0.05465243366213276555 ) ) ;
#11808 = EDGE_CURVE ( 'NONE', #966, #13820, #17269, .T. ) ;
#11809 = DIRECTION ( 'NONE',  ( -0.1060008583745224581, 0.000000000000000000, -0.9943660382494288186 ) ) ;
#11810 = CARTESIAN_POINT ( 'NONE',  ( -14.39647200192898779, -1.983739999999848624, -9.747027169376975664 ) ) ;
#11811 = CIRCLE ( 'NONE', #9686, 30.16249999999999787 ) ;
#11812 = LINE ( 'NONE', #3404, #16449 ) ;
#11813 = CARTESIAN_POINT ( 'NONE',  ( 1.660370454735925483, 15.04581296003263446, -0.5192195669560754068 ) ) ;
#11814 = ORIENTED_EDGE ( 'NONE', *, *, #15294, .F. ) ;
#11815 = LINE ( 'NONE', #1850, #13904 ) ;
#11816 = DIRECTION ( 'NONE',  ( 0.9966381950048638361, 0.000000000000000000, -0.08192867786951699149 ) ) ;
#11817 = DIRECTION ( 'NONE',  ( 1.000000000000000000, 0.000000000000000000, 0.000000000000000000 ) ) ;
#11818 = LINE ( 'NONE', #5165, #18403 ) ;
#11820 = CARTESIAN_POINT ( 'NONE',  ( 19.72286286404087363, -3.871483444068603230, -14.16070975014500632 ) ) ;
#11819 = DIRECTION ( 'NONE',  ( 0.000000000000000000, 0.000000000000000000, 1.000000000000000000 ) ) ;
#11821 = ORIENTED_EDGE ( 'NONE', *, *, #1891, .F. ) ;
#11822 = EDGE_LOOP ( 'NONE', ( #18936, #17794 ) ) ;
#11823 = CARTESIAN_POINT ( 'NONE',  ( 5.522956963460583957, 13.98659666219624675, -0.8314415007726022599 ) ) ;
#11824 = CARTESIAN_POINT ( 'NONE',  ( 2.520748753591570690, 25.39269750000000059, -24.56335908395234924 ) ) ;
#11825 = AXIS2_PLACEMENT_3D ( 'NONE', #17737, #17285, #7122 ) ;
#11826 = ORIENTED_EDGE ( 'NONE', *, *, #14416, .T. ) ;
#11827 = VERTEX_POINT ( 'NONE', #1740 ) ;
#11828 = CARTESIAN_POINT ( 'NONE',  ( 12.79472653632228507, -1.983739999999999393, -13.31637763425449883 ) ) ;
#11829 = EDGE_LOOP ( 'NONE', ( #17002, #11246, #21403, #21210 ) ) ;
#11830 = EDGE_CURVE ( 'NONE', #7786, #13109, #20297, .T. ) ;
#11831 = CARTESIAN_POINT ( 'NONE',  ( 8.448334465459019782, 11.54763819966888150, 2.948056682048101340 ) ) ;
#11832 = LINE ( 'NONE', #2306, #4234 ) ;
#11833 = EDGE_CURVE ( 'NONE', #20277, #3371, #17983, .T. ) ;
#11834 = DIRECTION ( 'NONE',  ( 0.000000000000000000, 1.000000000000000000, 0.000000000000000000 ) ) ;
#11835 = CARTESIAN_POINT ( 'NONE',  ( 3.360635606688116894, 36.51313500000000545, -20.45316710734507026 ) ) ;
#11836 = CARTESIAN_POINT ( 'NONE',  ( -0.07141578697956746380, 17.27597877604544863, 0.1156807881660063680 ) ) ;
#11837 = DIRECTION ( 'NONE',  ( -0.2868778675745010664, 0.000000000000000000, -0.9579671649362032637 ) ) ;
#11838 = ORIENTED_EDGE ( 'NONE', *, *, #9120, .F. ) ;
#11839 = CARTESIAN_POINT ( 'NONE',  ( 4.036164809125949660, 12.82285234092424098, 0.8599284710103052287 ) ) ;
#11840 = CARTESIAN_POINT ( 'NONE',  ( 46.03750000000000142, -9.531985000000000596, -10.31874999999999964 ) ) ;
#11841 = CARTESIAN_POINT ( 'NONE',  ( 53.54886731469894556, -5.294027063544084477, -16.17778660901759125 ) ) ;
#11842 = LINE ( 'NONE', #15286, #16671 ) ;
#11843 = VECTOR ( 'NONE', #12244, 1000.000000000000000 ) ;
#11844 = CARTESIAN_POINT ( 'NONE',  ( 29.22749461619170219, -5.959792500000001603, -4.986088976786413163 ) ) ;
#11845 = ORIENTED_EDGE ( 'NONE', *, *, #1834, .T. ) ;
#11846 = CARTESIAN_POINT ( 'NONE',  ( 5.497918191286784939, 19.19176664446208136, -1.343533416796099944 ) ) ;
#11847 = CARTESIAN_POINT ( 'NONE',  ( 12.82008979290802309, 19.79331256264924832, 6.077639648942910533 ) ) ;
#11848 = ORIENTED_EDGE ( 'NONE', *, *, #19377, .T. ) ;
#11849 = CARTESIAN_POINT ( 'NONE',  ( 9.359056336617545213, 17.47150019132489263, 7.876253759257760834 ) ) ;
#11850 = CARTESIAN_POINT ( 'NONE',  ( 2.863177793647310843, 19.21875272216368202, 7.432696887173809053 ) ) ;
#11851 = DIRECTION ( 'NONE',  ( 0.000000000000000000, -1.000000000000000000, -0.000000000000000000 ) ) ;
#11852 = EDGE_CURVE ( 'NONE', #15164, #15141, #11965, .T. ) ;
#11853 = CARTESIAN_POINT ( 'NONE',  ( 12.88040283537677588, 38.48766750000000059, -0.09070320285213756550 ) ) ;
#11854 = CARTESIAN_POINT ( 'NONE',  ( 7.320120958300368130, 15.63209079431325144, 7.583971929050274063 ) ) ;
#11855 = EDGE_CURVE ( 'NONE', #17362, #19935, #18760, .T. ) ;
#11856 = DIRECTION ( 'NONE',  ( -0.7776383362760928009, 0.000000000000000000, 0.6287118719681937806 ) ) ;
#11857 = VECTOR ( 'NONE', #20128, 1000.000000000000000 ) ;
#11858 = CARTESIAN_POINT ( 'NONE',  ( 14.23150068160818726, 21.00494883119180045, 3.295237727640887293 ) ) ;
#11859 = CARTESIAN_POINT ( 'NONE',  ( 5.099963284237507111, 11.34514690749418087, 5.595862192416997338 ) ) ;
#11860 = DIRECTION ( 'NONE',  ( 0.1060008583745224581, 0.000000000000000000, 0.9943660382494288186 ) ) ;
#11861 = DIRECTION ( 'NONE',  ( 0.000000000000000000, 1.000000000000000000, 0.000000000000000000 ) ) ;
#11862 = CARTESIAN_POINT ( 'NONE',  ( 46.03750000000000142, -3.968114999999999615, -10.31874999999999964 ) ) ;
#11863 = DIRECTION ( 'NONE',  ( -0.3140771401027084853, 0.9459569826691583971, -0.08075231887918268847 ) ) ;
#11864 = CARTESIAN_POINT ( 'NONE',  ( -160.2647810241784896, 30.56064500000000095, 10.71562489836746046 ) ) ;
#11865 = CARTESIAN_POINT ( 'NONE',  ( 10.72442325415146946, -2.948066920625321607, -17.12250937314169974 ) ) ;
#11866 = SURFACE_SIDE_STYLE ('',( #2123 ) ) ;
#11867 = ORIENTED_EDGE ( 'NONE', *, *, #2107, .T. ) ;
#11868 = DIRECTION ( 'NONE',  ( 0.000000000000000000, -1.000000000000000000, -0.000000000000000000 ) ) ;
#11869 = B_SPLINE_CURVE_WITH_KNOTS ( 'NONE', 3,
 ( #10729, #2317, #7519, #19331, #880, #2207, #4196, #14175, #9051, #7401, #12714, #14490, #12277, #20880, #5750, #10615, #7948, #14823, #8272, #8052, #3192, #14718, #2755, #21652, #12837, #11381 ),
 .UNSPECIFIED., .F., .F.,
 ( 4, 2, 2, 1, 2, 2, 2, 2, 1, 2, 2, 2, 2, 4 ),
 ( 0.000000000000000000, 0.06249999999999777955, 0.1249999999999955591, 0.1874999999999933387, 0.2187499999999900913, 0.2499999999999868439, 0.5000000000000003331, 0.6250000000000033307, 0.6875000000000076605, 0.7187500000000097700, 0.7500000000000117684, 0.8125000000000098810, 0.8750000000000079936, 1.000000000000000000 ),
 .UNSPECIFIED. ) ;
#11870 = CARTESIAN_POINT ( 'NONE',  ( 8.610469691664995651, 21.47961674228977103, 0.3618051172526235981 ) ) ;
#11871 = FACE_OUTER_BOUND ( 'NONE', #10382, .T. ) ;
#11872 = VERTEX_POINT ( 'NONE', #3742 ) ;
#11873 = CARTESIAN_POINT ( 'NONE',  ( 13.04877617004700951, 13.26865620857769201, 5.423244249217728630 ) ) ;
#11874 = CARTESIAN_POINT ( 'NONE',  ( 29.45491884992628329, 34.52875999999999834, -15.58809351040512325 ) ) ;
#11876 = DIRECTION ( 'NONE',  ( -0.000000000000000000, -1.000000000000000000, 0.000000000000000000 ) ) ;
#11875 = CARTESIAN_POINT ( 'NONE',  ( 2.607742312338097168, 20.27761254839711924, 2.237459158246773328 ) ) ;
#11877 = APPLICATION_CONTEXT ( 'automotive_design' ) ;
#11878 = EDGE_LOOP ( 'NONE', ( #20937, #21634, #21638, #9841, #13781, #3920 ) ) ;
#11879 = DIRECTION ( 'NONE',  ( 0.000000000000000000, 0.000000000000000000, 1.000000000000000000 ) ) ;
#11880 = EDGE_CURVE ( 'NONE', #11521, #21727, #4285, .T. ) ;
#11881 = CARTESIAN_POINT ( 'NONE',  ( 16.85197508397059707, 19.43957250000000059, -16.77951971243562923 ) ) ;
#11882 = EDGE_LOOP ( 'NONE', ( #7027, #13233, #740, #1339, #7201, #2147, #6157, #16795, #16772, #4779, #20930, #18671 ) ) ;
#11883 = CARTESIAN_POINT ( 'NONE',  ( 9.167756006212099962, 13.35056178516542325, 6.341038218456379383 ) ) ;
#11884 = EDGE_CURVE ( 'NONE', #10927, #10018, #19534, .T. ) ;
#11885 = CARTESIAN_POINT ( 'NONE',  ( 11.15100426632415420, 14.44107328295670634, -3.341937556964096334 ) ) ;
#11886 = CARTESIAN_POINT ( 'NONE',  ( 4.017631021903100397, 15.51072843360936204, -1.195195369806848262 ) ) ;
#11887 = CARTESIAN_POINT ( 'NONE',  ( 9.448052803682784884, 16.63233464712778087, 8.098436675483521086 ) ) ;
#11888 = CARTESIAN_POINT ( 'NONE',  ( 16.78551053486653544, -7.162656031619696329, -15.91463781719514081 ) ) ;
#11889 = CARTESIAN_POINT ( 'NONE',  ( 52.44708915697334106, -1.983739999999999837, 4.020247972991190188 ) ) ;
#11890 = AXIS2_PLACEMENT_3D ( 'NONE', #19444, #5853, #9389 ) ;
#11891 = VERTEX_POINT ( 'NONE', #15916 ) ;
#11892 = CARTESIAN_POINT ( 'NONE',  ( 8.946817783206428842, 20.96102289200085167, 1.313562465597416740 ) ) ;
#11893 = CARTESIAN_POINT ( 'NONE',  ( 12.16871400957597515, 21.60439101236092085, -1.553992429234034800 ) ) ;
#11894 = ORIENTED_EDGE ( 'NONE', *, *, #13068, .T. ) ;
#11895 = ORIENTED_EDGE ( 'NONE', *, *, #17551, .F. ) ;
#11896 = DIRECTION ( 'NONE',  ( 0.000000000000000000, 1.000000000000000000, 0.000000000000000000 ) ) ;
#11897 = CARTESIAN_POINT ( 'NONE',  ( 10.94956279435578139, 14.20305175510790185, -3.949782705418857454 ) ) ;
#11899 = CARTESIAN_POINT ( 'NONE',  ( 49.72033008250774344, -9.531985000000000596, -2.687827786179598277 ) ) ;
#11898 = CARTESIAN_POINT ( 'NONE',  ( 2.526745181667069406, 20.84690199368946040, 1.966986596898897544 ) ) ;
#11900 = ORIENTED_EDGE ( 'NONE', *, *, #11272, .T. ) ;
#11901 = CARTESIAN_POINT ( 'NONE',  ( 7.175445692564514921, 18.81307093152634735, 7.806506937020126102 ) ) ;
#11902 = EDGE_CURVE ( 'NONE', #11247, #18443, #16125, .T. ) ;
#11903 = CARTESIAN_POINT ( 'NONE',  ( 64.66604708500285881, 34.52875999999999834, -11.54913207920052720 ) ) ;
#11904 = ORIENTED_EDGE ( 'NONE', *, *, #4044, .T. ) ;
#11905 = CARTESIAN_POINT ( 'NONE',  ( -24.21104940531825633, 43.41875999999999891, -25.29232732678598339 ) ) ;
#11906 = ORIENTED_EDGE ( 'NONE', *, *, #15494, .F. ) ;
#11907 = CARTESIAN_POINT ( 'NONE',  ( 20.22951472560300346, -1.344520626714845069, -14.75553331646387711 ) ) ;
#11908 = DIRECTION ( 'NONE',  ( -0.1060008583745200572, 0.000000000000000000, -0.9943660382494290406 ) ) ;
#11909 = CARTESIAN_POINT ( 'NONE',  ( -29.36874999999999858, 23.41816500000000190, 0.000000000000000000 ) ) ;
#11910 = CARTESIAN_POINT ( 'NONE',  ( 2.035270604800319738, 12.09972725174282182, 1.536988627584183309 ) ) ;
#11911 = FACE_OUTER_BOUND ( 'NONE', #20306, .T. ) ;
#11912 = VERTEX_POINT ( 'NONE', #10914 ) ;
#11913 = LINE ( 'NONE', #15142, #2227 ) ;
#11914 = DIRECTION ( 'NONE',  ( 0.9037041334408600912, 0.3596272420165190775, 0.2323512126103423614 ) ) ;
#11915 = EDGE_CURVE ( 'NONE', #1449, #6627, #8079, .T. ) ;
#11916 = DIRECTION ( 'NONE',  ( 0.000000000000000000, 0.000000000000000000, 1.000000000000000000 ) ) ;
#11918 = CARTESIAN_POINT ( 'NONE',  ( 18.74736864250175472, -5.850096548006167296, -14.30666788301311954 ) ) ;
#11917 = CYLINDRICAL_SURFACE ( 'NONE', #12335, 3.175000000000000711 ) ;
#11919 = EDGE_LOOP ( 'NONE', ( #19096, #5827, #8924, #1310, #16483 ) ) ;
#11920 = ORIENTED_EDGE ( 'NONE', *, *, #18355, .F. ) ;
#11921 = CARTESIAN_POINT ( 'NONE',  ( 10.82096220742486281, 16.27085401118791452, -3.689681977176763716 ) ) ;
#11922 = VECTOR ( 'NONE', #10273, 1000.000000000000000 ) ;
#11923 = CARTESIAN_POINT ( 'NONE',  ( 0.07032913840789803417, 12.52705325500010325, 1.657397282339138078 ) ) ;
#11924 = ORIENTED_EDGE ( 'NONE', *, *, #8819, .T. ) ;
#11925 = ORIENTED_EDGE ( 'NONE', *, *, #20042, .T. ) ;
#11926 = CARTESIAN_POINT ( 'NONE',  ( 42.27821610176829381, 34.52875999999999834, 7.496956594510385763 ) ) ;
#11927 = EDGE_CURVE ( 'NONE', #1721, #20753, #10911, .T. ) ;
#11928 = ORIENTED_EDGE ( 'NONE', *, *, #21140, .F. ) ;
#11929 = ADVANCED_FACE ( 'NONE', ( #2293 ), #4400, .T. ) ;
#11930 = CARTESIAN_POINT ( 'NONE',  ( 7.447672119940222935, 15.77891879107950324, -2.094525022072177833 ) ) ;
#11931 = AXIS2_PLACEMENT_3D ( 'NONE', #1567, #6757, #342 ) ;
#11932 = LINE ( 'NONE', #13291, #3669 ) ;
#11933 = FACE_OUTER_BOUND ( 'NONE', #6864, .T. ) ;
#11934 = PLANE ( 'NONE',  #15735 ) ;
#11935 = CARTESIAN_POINT ( 'NONE',  ( -0.1907120674000438720, 14.86661835102559159, 0.2656455004388350027 ) ) ;
#11936 = LINE ( 'NONE', #18666, #15117 ) ;
#11937 = ORIENTED_EDGE ( 'NONE', *, *, #19993, .T. ) ;
#11938 = CARTESIAN_POINT ( 'NONE',  ( 30.97944403357121956, 0.000000000000000000, -8.103300075789407586 ) ) ;
#11939 = CARTESIAN_POINT ( 'NONE',  ( 0.4090325377308574040, 17.21628798890151302, 0.6179089441262706206 ) ) ;
#11940 = DIRECTION ( 'NONE',  ( -0.2868778675745008999, 0.000000000000000000, -0.9579671649362034858 ) ) ;
#11941 = CARTESIAN_POINT ( 'NONE',  ( 53.35716956354660567, -5.185007377690430630, -16.41558412949913404 ) ) ;
#11942 = DIRECTION ( 'NONE',  ( -0.9488823340533351081, 0.2002559181062071036, -0.2439669719140995230 ) ) ;
#11943 = EDGE_CURVE ( 'NONE', #9466, #16242, #10210, .T. ) ;
#11944 = FACE_OUTER_BOUND ( 'NONE', #6041, .T. ) ;
#11945 = ORIENTED_EDGE ( 'NONE', *, *, #19853, .F. ) ;
#11946 = CARTESIAN_POINT ( 'NONE',  ( 9.052467241478945326, 12.91190710784102080, 6.975301435476066736 ) ) ;
#11947 = CARTESIAN_POINT ( 'NONE',  ( 39.42154620619644589, -7.547609999999999708, -4.343957374020581241 ) ) ;
#11948 = CARTESIAN_POINT ( 'NONE',  ( 13.37137086141695619, 16.12366711453539736, 7.173766633443349860 ) ) ;
#11949 = ORIENTED_EDGE ( 'NONE', *, *, #3020, .F. ) ;
#11950 = ORIENTED_EDGE ( 'NONE', *, *, #9301, .F. ) ;
#11951 = CARTESIAN_POINT ( 'NONE',  ( 13.11605872809629858, 21.42344080416877006, 1.163243345628418357 ) ) ;
#11952 = CARTESIAN_POINT ( 'NONE',  ( 9.491314998020746074, 14.79089830327174937, 7.774602169083346226 ) ) ;
#11953 = CARTESIAN_POINT ( 'NONE',  ( 4.255350674082147400, 12.02975038249582163, 2.250507228818958705 ) ) ;
#11954 = CARTESIAN_POINT ( 'NONE',  ( 59.61686353177688602, -3.968114999999999615, -0.7993558564620834028 ) ) ;
#11955 = ADVANCED_FACE ( 'NONE', ( #19309 ), #5602, .F. ) ;
#11956 = DIRECTION ( 'NONE',  ( 0.000000000000000000, -1.000000000000000000, 0.000000000000000000 ) ) ;
#11957 = CARTESIAN_POINT ( 'NONE',  ( 1.414909354815941267, 18.54739417496245579, 8.316710155238244084 ) ) ;
#11958 = CARTESIAN_POINT ( 'NONE',  ( 1.026903634312197333, 19.93157197858078788, 2.808439018299325074 ) ) ;
#11959 = DIRECTION ( 'NONE',  ( -0.6287118719681937806, 0.000000000000000000, -0.7776383362760928009 ) ) ;
#11960 = ADVANCED_FACE ( 'NONE', ( #10704, #7702 ), #12362, .T. ) ;
#11961 = CARTESIAN_POINT ( 'NONE',  ( 29.37436411451823304, 31.72299998434776569, 10.71597283099095499 ) ) ;
#11962 = CARTESIAN_POINT ( 'NONE',  ( 11.73734890072733172, 21.76139788190002022, 1.882179297186191036 ) ) ;
#11963 = CARTESIAN_POINT ( 'NONE',  ( 4.677500656696262915, 10.96673477554678122, 3.790603218585762324 ) ) ;
#11964 = DIRECTION ( 'NONE',  ( 0.08420877549337300871, 0.000000000000000000, 0.9964481331860212121 ) ) ;
#11965 = CIRCLE ( 'NONE', #16231, 1.191259999999998209 ) ;
#11966 = CARTESIAN_POINT ( 'NONE',  ( 20.22718371673215287, -1.176379440366829954, -14.75900186987939300 ) ) ;
#11967 = CARTESIAN_POINT ( 'NONE',  ( 6.416266621286034422, 10.92343542074206120, 2.783831947462576561 ) ) ;
#11968 = LINE ( 'NONE', #18699, #10242 ) ;
#11969 = DIRECTION ( 'NONE',  ( 1.000000000000000000, 0.000000000000000000, 0.000000000000000000 ) ) ;
#11970 = CARTESIAN_POINT ( 'NONE',  ( 10.72528277947465014, -3.117068478670475429, -17.12846307055972872 ) ) ;
#11971 = EDGE_CURVE ( 'NONE', #8930, #1068, #2455, .T. ) ;
#11972 = EDGE_CURVE ( 'NONE', #9795, #13402, #17663, .T. ) ;
#11973 = CARTESIAN_POINT ( 'NONE',  ( -17.46249999999999858, 32.54247999999999763, 0.000000000000000000 ) ) ;
#11974 = ADVANCED_FACE ( 'NONE', ( #4042 ), #17752, .F. ) ;
#11975 = DIRECTION ( 'NONE',  ( -0.7421532822901580895, 0.000000000000000000, 0.6702301885068630005 ) ) ;
#11976 = CARTESIAN_POINT ( 'NONE',  ( 11.28778781650649776, 17.64863795527461576, 7.430186115869990893 ) ) ;
#11977 = VECTOR ( 'NONE', #12876, 1000.000000000000000 ) ;
#11978 = ORIENTED_EDGE ( 'NONE', *, *, #7088, .T. ) ;
#11979 = CARTESIAN_POINT ( 'NONE',  ( 13.16590010066154015, 14.90344756276430616, 6.212949255494740974 ) ) ;
#11980 = CARTESIAN_POINT ( 'NONE',  ( 26.59062499999999929, 26.59189500000000095, 10.71562499999999929 ) ) ;
#11982 = DIRECTION ( 'NONE',  ( 0.000000000000000000, 1.000000000000000000, 0.000000000000000000 ) ) ;
#11981 = CARTESIAN_POINT ( 'NONE',  ( 0.5001283093862811668, 19.74033803598106118, 2.301173850479345528 ) ) ;
#11983 = ORIENTED_EDGE ( 'NONE', *, *, #16573, .F. ) ;
#11984 = DIRECTION ( 'NONE',  ( 0.000000000000000000, 0.000000000000000000, 1.000000000000000000 ) ) ;
#11985 = CARTESIAN_POINT ( 'NONE',  ( 46.03750000000000142, -1.983739999999999393, -10.31874999999999964 ) ) ;
#11986 = DIRECTION ( 'NONE',  ( 0.000000000000000000, 0.000000000000000000, 1.000000000000000000 ) ) ;
#11987 = AXIS2_PLACEMENT_3D ( 'NONE', #528, #7277, #14038 ) ;
#11988 = CARTESIAN_POINT ( 'NONE',  ( 52.50728002481341150, 38.88803500000000213, -18.54895932800084779 ) ) ;
#11989 = VECTOR ( 'NONE', #14238, 1000.000000000000000 ) ;
#11990 = ORIENTED_EDGE ( 'NONE', *, *, #21038, .T. ) ;
#11991 = CARTESIAN_POINT ( 'NONE',  ( 9.709978852237810543, 21.05303134726939973, 3.417248539804212282 ) ) ;
#11992 = CARTESIAN_POINT ( 'NONE',  ( 3.930841689390241811, 20.49042122551175638, 4.838430134900644219 ) ) ;
#11993 = AXIS2_PLACEMENT_3D ( 'NONE', #15877, #7450, #20941 ) ;
#11994 = CARTESIAN_POINT ( 'NONE',  ( 7.553652573848785856, 21.00575954651474220, 3.188648499624214150 ) ) ;
#11995 = CARTESIAN_POINT ( 'NONE',  ( 9.442279758265636147, 19.32856220366442201, -2.967836764750759304 ) ) ;
#11996 = FACE_OUTER_BOUND ( 'NONE', #8813, .T. ) ;
#11997 = EDGE_CURVE ( 'NONE', #21211, #6484, #20147, .T. ) ;
#11998 = CARTESIAN_POINT ( 'NONE',  ( 30.78626241496060700, 32.52628750000000224, -2.552201779827368622 ) ) ;
#11999 = VERTEX_POINT ( 'NONE', #12453 ) ;
#12000 = CARTESIAN_POINT ( 'NONE',  ( 9.180768457294835372, 21.06661498530921151, 1.940146591543385979 ) ) ;
#12001 = CARTESIAN_POINT ( 'NONE',  ( 12.94877351110852715, 11.26870765665696084, 4.634005384042424680 ) ) ;
#12002 = ORIENTED_EDGE ( 'NONE', *, *, #18927, .F. ) ;
#12003 = CARTESIAN_POINT ( 'NONE',  ( -17.46249999999999858, 33.73373999999999739, 0.000000000000000000 ) ) ;
#12004 = DIRECTION ( 'NONE',  ( 0.9790635044817342925, 0.000000000000000000, -0.2035550397114870569 ) ) ;
#12005 = AXIS2_PLACEMENT_3D ( 'NONE', #903, #17830, #16279 ) ;
#12007 = LINE ( 'NONE', #18738, #15553 ) ;
#12006 = CARTESIAN_POINT ( 'NONE',  ( 2.950312850434896106, 11.97425653754774189, 6.932220074007259036 ) ) ;
#12008 = VERTEX_POINT ( 'NONE', #20952 ) ;
#12009 = CARTESIAN_POINT ( 'NONE',  ( 7.406607808117615654, 13.05076105357039573, 7.314782732399700116 ) ) ;
#12010 = AXIS2_PLACEMENT_3D ( 'NONE', #16208, #17421, #5804 ) ;
#12011 = ORIENTED_EDGE ( 'NONE', *, *, #8149, .F. ) ;
#12012 = CARTESIAN_POINT ( 'NONE',  ( 0.2665283650859920916, 12.98379964877340775, 2.505562667629908535 ) ) ;
#12013 = PLANE ( 'NONE',  #3321 ) ;
#12014 = VERTEX_POINT ( 'NONE', #16002 ) ;
#12015 = CARTESIAN_POINT ( 'NONE',  ( 1.991330241149480873, 13.57173140902838782, 1.074079535782173300 ) ) ;
#12016 = CARTESIAN_POINT ( 'NONE',  ( 27.93207353965470574, 32.54502000000000095, -8.388685343514779902 ) ) ;
#12017 = CARTESIAN_POINT ( 'NONE',  ( 42.35466991749225940, -9.531985000000000596, -17.94967221382040279 ) ) ;
#12018 = AXIS2_PLACEMENT_3D ( 'NONE', #14231, #9215, #7572 ) ;
#12019 = LINE ( 'NONE', #7034, #20644 ) ;
#12020 = CARTESIAN_POINT ( 'NONE',  ( 4.690729861326075500, 20.36709625471669938, 6.894995340168590836 ) ) ;
#12021 = ADVANCED_FACE ( 'NONE', ( #17302 ), #7680, .F. ) ;
#12022 = DIRECTION ( 'NONE',  ( 0.000000000000000000, -1.000000000000000000, 0.000000000000000000 ) ) ;
#12023 = ORIENTED_EDGE ( 'NONE', *, *, #6278, .T. ) ;
#12024 = CARTESIAN_POINT ( 'NONE',  ( 37.29356535768673098, -6.356984999999999886, -6.700294045292300105 ) ) ;
#12025 = DIRECTION ( 'NONE',  ( 0.000000000000000000, 1.000000000000000000, 0.000000000000000000 ) ) ;
#12026 = DIRECTION ( 'NONE',  ( 0.000000000000000000, 1.000000000000000000, 0.000000000000000000 ) ) ;
#12028 = CARTESIAN_POINT ( 'NONE',  ( 13.42913409643213107, -6.549231401220326987, -15.39443542868764503 ) ) ;
#12027 = CARTESIAN_POINT ( 'NONE',  ( 30.74535937054756829, -3.968114999999999615, -3.684081112461307317 ) ) ;
#12029 = EDGE_LOOP ( 'NONE', ( #18222, #16718, #19009, #20087 ) ) ;
#12030 = EDGE_LOOP ( 'NONE', ( #7234, #18086, #9237, #18218 ) ) ;
#12031 = CARTESIAN_POINT ( 'NONE',  ( 10.20687392145870653, 20.34020649082646059, 4.946106562410360397 ) ) ;
#12032 = AXIS2_PLACEMENT_3D ( 'NONE', #7055, #21062, #10384 ) ;
#12034 = CARTESIAN_POINT ( 'NONE',  ( 31.04121718565060206, 0.000000000000000000, -8.720124554639784975 ) ) ;
#12033 = CARTESIAN_POINT ( 'NONE',  ( 2.107350683505484490, 11.83412605131448103, 1.752489760913824579 ) ) ;
#12035 = AXIS2_PLACEMENT_3D ( 'NONE', #16131, #7814, #14592 ) ;
#12036 = EDGE_LOOP ( 'NONE', ( #17607, #20144, #5099, #18158 ) ) ;
#12037 = VERTEX_POINT ( 'NONE', #14440 ) ;
#12038 = CARTESIAN_POINT ( 'NONE',  ( 23.77193158452286781, 29.75832250000000201, -15.00033089984030887 ) ) ;
#12039 = VERTEX_POINT ( 'NONE', #17532 ) ;
#12040 = CIRCLE ( 'NONE', #14889, 0.7950200000000000600 ) ;
#12041 = CARTESIAN_POINT ( 'NONE',  ( 7.584943636950675305, 13.21535262572377611, -0.9819277678746927140 ) ) ;
#12042 = DIRECTION ( 'NONE',  ( 0.9964481331860212121, 0.000000000000000000, -0.08420877549337300871 ) ) ;
#12043 = ORIENTED_EDGE ( 'NONE', *, *, #3422, .F. ) ;
#12044 = VECTOR ( 'NONE', #1601, 1000.000000000000114 ) ;
#12045 = AXIS2_PLACEMENT_3D ( 'NONE', #2496, #4157, #9230 ) ;
#12046 = CIRCLE ( 'NONE', #15599, 0.5953125000000005773 ) ;
#12047 = CARTESIAN_POINT ( 'NONE',  ( -17.46249999999999858, 34.31794000000000011, 0.000000000000000000 ) ) ;
#12048 = DIRECTION ( 'NONE',  ( 0.8334497143791951279, 0.000000000000000000, 0.5525953072558960066 ) ) ;
#12049 = CARTESIAN_POINT ( 'NONE',  ( 28.56548256563643662, -14.84248999999999974, -12.12873025803960658 ) ) ;
#12050 = CARTESIAN_POINT ( 'NONE',  ( 2.190455368389823576, 21.01608119939916364, 5.860843236296549463 ) ) ;
#12051 = EDGE_CURVE ( 'NONE', #6063, #9888, #3933, .T. ) ;
#12052 = CYLINDRICAL_SURFACE ( 'NONE', #18980, 0.5080000000000014504 ) ;
#12053 = EDGE_CURVE ( 'NONE', #3464, #11708, #7391, .T. ) ;
#12054 = ORIENTED_EDGE ( 'NONE', *, *, #6904, .T. ) ;
#12055 = CARTESIAN_POINT ( 'NONE',  ( 2.483346228476034590, 12.45711053362852283, 2.021137222503261555 ) ) ;
#12056 = CARTESIAN_POINT ( 'NONE',  ( 49.72033008250774344, 32.54502000000000095, -2.687827786179598277 ) ) ;
#12057 = LINE ( 'NONE', #17026, #19128 ) ;
#12058 = SURFACE_STYLE_FILL_AREA ( #1654 ) ;
#12059 = DIRECTION ( 'NONE',  ( 0.4987171968201936645, 0.000000000000000000, -0.8667647648559603235 ) ) ;
#12060 = ORIENTED_EDGE ( 'NONE', *, *, #16028, .F. ) ;
#12061 = CARTESIAN_POINT ( 'NONE',  ( 11.45962687667246804, 20.25175440475918265, -3.101195653451903400 ) ) ;
#12062 = CARTESIAN_POINT ( 'NONE',  ( 3.805353748838121053, 34.52875999999999834, -22.18284873352824960 ) ) ;
#12063 = CARTESIAN_POINT ( 'NONE',  ( 13.38710885774181314, 15.59940030760539820, 7.127019235770691630 ) ) ;
#12064 = EDGE_LOOP ( 'NONE', ( #13007, #957, #11867, #7076 ) ) ;
#12065 = VERTEX_POINT ( 'NONE', #2380 ) ;
#12066 = CARTESIAN_POINT ( 'NONE',  ( 1.998220421679061776, 25.39269750000000059, -22.64748046904500356 ) ) ;
#12067 = AXIS2_PLACEMENT_3D ( 'NONE', #1874, #15609, #8620 ) ;
#12068 = AXIS2_PLACEMENT_3D ( 'NONE', #5523, #20664, #13847 ) ;
#12069 = CARTESIAN_POINT ( 'NONE',  ( 9.327916374733275617, 17.71149373539732252, 7.821919058577349482 ) ) ;
#12070 = CARTESIAN_POINT ( 'NONE',  ( 4.550724514086687655, 19.87742190051230295, 6.393129328018801516 ) ) ;
#12071 = CARTESIAN_POINT ( 'NONE',  ( 54.55586098912687731, 32.54502000000000095, -6.056925149195119040 ) ) ;
#12072 = CARTESIAN_POINT ( 'NONE',  ( 5.710684426658359847, 17.22355540511336258, -1.322581421157464909 ) ) ;
#12073 = CARTESIAN_POINT ( 'NONE',  ( 7.068676109993910828, 17.98782383223260695, 7.330006056139382942 ) ) ;
#12074 = CIRCLE ( 'NONE', #9929, 9.525000000000002132 ) ;
#12075 = FACE_OUTER_BOUND ( 'NONE', #5050, .T. ) ;
#12076 = ADVANCED_FACE ( 'NONE', ( #6012 ), #7254, .F. ) ;
#12077 = CARTESIAN_POINT ( 'NONE',  ( 7.701365284815051560, 12.68409469243044363, -1.677233022421109832 ) ) ;
#12078 = VECTOR ( 'NONE', #1196, 1000.000000000000114 ) ;
#12079 = CARTESIAN_POINT ( 'NONE',  ( 38.94885947252404179, -5.166721542084396823, -3.956611957468594287 ) ) ;
#12080 = CARTESIAN_POINT ( 'NONE',  ( 5.716420248627351874, 15.64056738454816120, 8.837994797662030777 ) ) ;
#12081 = DIRECTION ( 'NONE',  ( 0.8609107660235850723, 0.000000000000000000, -0.5087559856598092844 ) ) ;
#12082 = MECHANICAL_DESIGN_GEOMETRIC_PRESENTATION_REPRESENTATION (  '', ( #2139 ), #7487 ) ;
#12083 = ADVANCED_FACE ( 'NONE', ( #2150 ), #17424, .T. ) ;
#12084 = VECTOR ( 'NONE', #17340, 1000.000000000000000 ) ;
#12085 = EDGE_CURVE ( 'NONE', #14379, #17300, #10997, .T. ) ;
#12086 = CARTESIAN_POINT ( 'NONE',  ( -3.929154139288399961, 9.129395000000000593, 0.9374890779182719625 ) ) ;
#12087 = CARTESIAN_POINT ( 'NONE',  ( 0.1697664307767892677, 13.13563057234646081, 2.183769842644804005 ) ) ;
#12088 = DIRECTION ( 'NONE',  ( 0.000000000000000000, 1.000000000000000000, 0.000000000000000000 ) ) ;
#12089 = CARTESIAN_POINT ( 'NONE',  ( 10.73605050800646943, -2.562123915646048022, -17.10540653823293766 ) ) ;
#12090 = LINE ( 'NONE', #358, #6746 ) ;
#12091 = VECTOR ( 'NONE', #7168, 1000.000000000000114 ) ;
#12092 = B_SPLINE_CURVE_WITH_KNOTS ( 'NONE', 3,
 ( #6438, #4787, #11629, #6644, #3781, #12291, #8964, #1888, #13742, #17490, #5648, #5766, #15628, #20785, #2225, #19016, #19134, #12407, #2105, #5307, #20560, #10515, #20898, #15741, #12186, #4002, #10846, #3892, #19246, #569, #12522, #344, #13858, #15842, #7418, #7089, #15411, #4107, #6974, #5421, #10745, #18910, #5532, #8847, #17261, #14077, #8635, #14190, #233, #20438, #10414, #12072, #10630, #18800, #2333, #9067, #465, #3668, #7213, #13975, #20672, #17382, #671, #7313, #17156, #1995, #8737, #15514, #4536, #12623, #14506, #12731, #4328, #19345, #7534, #1106, #4213, #4440, #21221, #9289, #5964, #12961, #7743, #14298, #2557, #5864, #9613, #6080, #21334, #7850, #11276, #17705, #11067, #11170, #14731, #14626, #10951, #16064, #19453, #9398, #21438, #12854, #897, #4649, #9505, #1218, #7962, #17594, #6291, #19668, #7638, #14400, #18026, #21113, #17823, #2882, #2667, #13067, #9174, #2447, #786, #993, #16166, #19573, #17922, #2768, #16276, #21017, #6194, #19774, #16380, #15955, #20209, #8381, #4761, #13492, #9723, #11717, #20310, #16902, #6734, #19992, #3324, #4864, #9823, #18240, #3204, #21876, #98, #19889, #14949, #6848, #11605, #4963, #11393, #20096, #15271, #1750, #1429, #13608, #9938, #6621, #21549, #5080, #15155, #10156, #21667, #18341, #18139, #2997, #10055, #16487, #6527, #16701, #18452, #1542, #1320, #8287, #16805, #8491, #1642, #21769, #11831, #18560, #3423, #8063, #14834, #15057, #6408, #13180, #13385, #11497, #3099, #16591, #8172, #13287, #5505, #18885, #17131, #20530, #10601, #12376, #3755, #20758, #8816, #7288, #5278, #18771, #2196, #15713, #12041, #18659, #540, #3528, #3641, #12266, #5397, #10265, #13713, #8608, #8936, #5615, #14052, #5179, #11930, #10387, #15383, #15594, #17011, #1866, #207, #429, #1971, #10490, #7182, #13946, #8711, #6950, #20413, #15489, #315, #12160, #7060, #13826, #17232, #18988, #17348, #2074, #3863, #20643, #1387, #18620, #16553, #8350, #6911, #15121, #1500, #5037, #16768, #20054, #9892, #11788, #8129, #16657, #10015, #6692, #5239, #11892, #18302, #13564, #6485, #3160, #9784, #12000, #13249, #11672, #16865, #18411, #8246, #15018, #1607, #20160, #14908, #13452, #1710, #13674, #21838, #20374, #3282, #19958, #21736, #18520, #4830, #3487, #21624, #3386, #11565, #20268, #50, #1820, #13350, #10223, #6589, #10119, #4924, #8449, #15222, #3061, #6804, #5140, #16970, #8563, #15339, #168, #7252, #3820, #8774, #9004, #5806, #2378, #15886, #18843, #18947, #10675, #711, #606, #12119, #7014, #20715, #4039, #18732, #10785, #1929, #15447, #386, #274, #20487, #7139, #6457, #10198, #1792, #1474, #6774, #11537, #3253, #16941, #1584, #8535, #4698, #6337, #18277, #8328, #6662, #13423, #5011, #11765, #8777, #9109, #15783, #12122, #13910, #10681, #9222, #15891, #390, #17534, #10455, #7144, #13785, #16005, #17193, #15676, #20827, #506, #5466, #20608, #20720, #2382, #17637, #15558, #10558, #10889, #19060, #2490, #7257, #2033, #12228, #14016, #18951, #7466, #20490, #2269, #3824, #716, #4045, #5811, #17304, #5575, #7017, #5361, #5696, #17427, #14122, #18847, #3714, #14237, #10789, #2152, #12334, #20954, #7355, #9008, #12567, #19289, #3935, #8897, #610, #4151, #12456, #19179, #6128, #19712, #9764, #11216, #18187, #7897, #4702, #21159, #12786, #14775, #6340, #6014, #14340, #19827, #9442, #2603, #12668, #6234, #17756, #9551, #19613, #5906, #19509, #18077, #12898, #19391, #7683, #10999, #21484, #17967, #4585, #13008, #16430, #936, #16214, #16320, #11443, #11326, #16106, #14442, #17863, #11112, #4479, #2817, #4373, #832, #14673, #13114, #3040, #7578, #21055, #2937, #2709, #1041, #1262, #7787, #14555, #8003, #21273, #4260, #1158, #21380, #9663, #21813, #14998, #18495, #8330, #11648, #1477, #6462, #8224, #13651, #3141, #16945, #3468, #13542, #9865, #18600, #14882, #16844, #3577, #16530, #19936, #3256, #8424, #9992, #21714, #6568, #15098, #5123, #5221, #16634, #20032, #11979, #16747, #10098, #1361, #3367, #20351, #6890, #13329, #1797, #8104, #11769, #4809, #11873, #20248, #15320, #4900, #1588, #21600, #13226, #15200, #11541, #18384, #6666, #1685, #13427, #18708, #20137, #28, #10202, #6779, #5014, #8540, #143, #18281, #13763, #7114, #14099, #20694, #20581, #15654, #4023, #19037, #19157, #5331, #7236, #5441, #20802, #5551, #10653, #12205, #7333, #19269, #12309, #5786, #17406, #14212, #8752, #363, #2355, #15863, #15533, #1906, #7436, #15426, #13883, #5669, #483, #252, #17281, #18928, #588, #12545, #692, #20926, #10316, #18821, #8652, #3910, #17061, #12429, #10767, #2126, #12097, #3798, #13994, #2246, #3688, #6992, #8983, #15761, #10431, #20462, #9085, #17171, #10534, #2011, #8870, #17510, #10867, #12981, #15979, #19689, #810, #16190, #7982, #1017, #2579, #19593, #17731, #7659, #6210, #11191, #14318, #14420, #11091, #7764, #21037, #11301, #5988, #21353, #12758, #19480, #2690, #21249, #9527, #1129, #2906, #14753, #21458, #15509, #17256, #8844, #11951, #2098, #5528, #17486 ),
 .UNSPECIFIED., .F., .F.,
 ( 4, 3, 3, 3, 3, 3, 3, 3, 3, 3, 3, 3, 3, 3, 3, 3, 3, 3, 3, 3, 3, 3, 3, 3, 3, 3, 3, 3, 3, 3, 3, 3, 3, 3, 3, 3, 3, 3, 3, 3, 3, 3, 3, 3, 3, 3, 3, 3, 3, 3, 3, 3, 3, 3, 3, 3, 3, 3, 3, 3, 3, 3, 3, 3, 3, 3, 3, 3, 3, 3, 3, 3, 3, 3, 3, 3, 3, 3, 3, 3, 3, 3, 3, 3, 3, 3, 3, 3, 3, 3, 3, 3, 3, 3, 3, 3, 3, 3, 3, 3, 3, 3, 3, 3, 3, 3, 3, 3, 3, 3, 3, 3, 3, 3, 3, 3, 3, 3, 3, 3, 3, 3, 3, 3, 3, 3, 3, 3, 3, 3, 3, 3, 3, 3, 3, 3, 3, 3, 3, 3, 3, 3, 3, 3, 3, 3, 3, 3, 3, 3, 3, 3, 3, 3, 3, 3, 3, 3, 3, 3, 3, 3, 3, 3, 3, 3, 3, 3, 3, 3, 3, 3, 3, 3, 3, 3, 3, 3, 3, 3, 3, 3, 3, 3, 3, 3, 3, 3, 3, 3, 3, 3, 3, 3, 3, 3, 3, 3, 3, 3, 3, 3, 3, 3, 3, 3, 3, 3, 3, 3, 3, 3, 3, 3, 3, 3, 4 ),
 ( 3.913411576274749967E-10, 0.006369427103560140052, 0.01249999939102700020, 0.01273885381577509988, 0.01910828052800209870, 0.02547770724021910030, 0.02875000254734080135, 0.03184713395243609496, 0.03821656066465310003, 0.04458598737687999997, 0.04500000225596059722, 0.05095541408909699810, 0.05732484080131399623, 0.06124999398789569838, 0.06369426751353099436, 0.07006369422575800532, 0.07643312093797499651, 0.07750000840243019551, 0.08280254765019190444, 0.08917197436240889563, 0.09374998978646680026, 0.09554140107463589271, 0.1019108277868729928, 0.1082802544991000038, 0.1100000129344189947, 0.1146496812113270009, 0.1210191079235540118, 0.1262499915749089874, 0.1273885346356810055, 0.1337579613479080165, 0.1401273880601349997, 0.1425000117241630171, 0.1464968147723620107, 0.1528662414845889939, 0.1587499967440479942, 0.1592356681968160048, 0.1656050949090429880, 0.1719745216212700267, 0.1750000048165079869, 0.1783439483334970099, 0.1847133750457240209, 0.1910828017579510041, 0.1912499997860669931, 0.1974522284701780150, 0.2038216551824049982, 0.2074999958526209942, 0.2101910818945320059, 0.2165605086067590168, 0.2229299353189860000, 0.2237500049592059947, 0.2292993620312130110, 0.2356687887434399942, 0.2399999896536270105, 0.2420382154556670051, 0.2484076421678940161, 0.2547770688801209715, 0.2562500107525759740, 0.2611464955923479825, 0.2675159223045749934, 0.2724999892630159959, 0.2738853490168020044, 0.2802547757290280162, 0.2866242024412549716, 0.2887500119236349749, 0.2929936291533819515, 0.2993630558656089624, 0.3049999937500470493, 0.3057324825778360289, 0.3121019092900629843, 0.3184713360022899953, 0.3212500068789819752, 0.3248407627145170062, 0.3312101894267439617, 0.3375796161389710281, 0.3439490428511979836, 0.3503184695634249946, 0.3537499981227409940, 0.3566878962756520055, 0.3630573229878790165, 0.3694267497001059719, 0.3700000016114870505, 0.3757961764122330073, 0.3821656031244600182, 0.3862499903775790111, 0.3885350298366869737, 0.3949044565489140401, 0.4012738832611409956, 0.4025000078859060082, 0.4076433099733680065, 0.4140127366855950175, 0.4187499876790780062, 0.4203821633978219729, 0.4267515901100490394, 0.4331210168222760504, 0.4350000112083169945, 0.4394904435345030058, 0.4458598702467300168, 0.4512499907420399747, 0.4522292969589570277, 0.4585987236710840076, 0.4649681503833110185, 0.4675000083970360376, 0.4713375770955380295, 0.4777070038077650405, 0.4837499959041640096, 0.4840764305199919959, 0.4904458572322190069, 0.4968152839444460178, 0.5000000005418490101, 0.5031847106566730288, 0.5095541373688999842, 0.5159235640811269397, 0.5162499986996510470, 0.5222929907933540061, 0.5286624175055810726, 0.5324999918453350300, 0.5350318442178080280, 0.5414012709300350945, 0.5477706976421620189, 0.5487500045795760117, 0.5541401243543889743, 0.5605095510666160408, 0.5649999869507580375, 0.5668789777788429962, 0.5732484044910699517, 0.5796178312032970181, 0.5812500095876119710, 0.5859872579155239736, 0.5923566846277509290, 0.5974999880555230680, 0.5987261113399779955, 0.6050955380522050620, 0.6114649647644320174, 0.6137500091740419883, 0.6178343914766590839, 0.6242038181888860393, 0.6299999931106780027, 0.6305732449010130747, 0.6369426716132400301, 0.6433120983254669856, 0.6462500028379470907, 0.6496815250376939410, 0.6560509517499210075, 0.6624203784621479629, 0.6687898051743739192, 0.6751592318866019848, 0.6787499938729660842, 0.6815286585988289403, 0.6878980853110550076, 0.6942675120232830732, 0.6950000011427179825, 0.7006369387355090295, 0.7070063654477359849, 0.7112499871106169325, 0.7133757921598630203, 0.7197452188720899757, 0.7261146455843170422, 0.7275000071637089949, 0.7324840722965439976, 0.7388534990087709531, 0.7437499859629570498, 0.7452229257209980195, 0.7515923524332249750, 0.7579617791454519304, 0.7600000090789329477, 0.7643312058576789969, 0.7707006325699060634, 0.7762499900630959182, 0.7770700592821330188, 0.7834394859943600853, 0.7898089127065870407, 0.7925000047482080312, 0.7961783394187139651, 0.8025477661309410315, 0.8087499948081490198, 0.8089171928431679870, 0.8152866195553949424, 0.8216560462676220089, 0.8249999962251529650, 0.8280254729798489643, 0.8343948996920759198, 0.8407643264043029863, 0.8412499979177490150, 0.8471337531165300527, 0.8535031798287568972, 0.8574999881000170410, 0.8598726065409840746, 0.8662420332532110301, 0.8726114599654379855, 0.8737500041287140640, 0.8789808866775650209, 0.8853503133897919763, 0.8899999846533520609, 0.8917197401020189318, 0.8980891668142459983, 0.9044585935264729537, 0.9062500080622120091, 0.9108280202386999092, 0.9171974469509269756, 0.9224999871212090641, 0.9235668736631539311, 0.9299363003753809975, 0.9363057270876080640, 0.9387500060427089732, 0.9426751537998350194, 0.9490445805120619749, 0.9549999923723109241, 0.9554140072242890414, 0.9617834339364159657, 0.9681528606486430322, 0.9712499985339340114, 0.9745222873608699876, 0.9808917140730969431, 0.9872611407853240095, 0.9874999952026149996, 0.9936305674975509650, 0.9999999942097779204 ),
 .UNSPECIFIED. ) ;
#12093 = FACE_OUTER_BOUND ( 'NONE', #2182, .T. ) ;
#12094 = CARTESIAN_POINT ( 'NONE',  ( 11.22444918248842072, 18.10120891158497258, 7.310595827509144051 ) ) ;
#12095 = CARTESIAN_POINT ( 'NONE',  ( 29.15193331460030279, -7.547927499999999235, -13.61707959051006966 ) ) ;
#12096 = CYLINDRICAL_SURFACE ( 'NONE', #6752, 1.191259999999999986 ) ;
#12097 = CARTESIAN_POINT ( 'NONE',  ( 11.15612707441398044, 15.87324431098740085, -3.568713840340196786 ) ) ;
#12098 = DIRECTION ( 'NONE',  ( 0.000000000000000000, 1.000000000000000000, 0.000000000000000000 ) ) ;
#12100 = DIRECTION ( 'NONE',  ( -0.6702301885068652210, 0.000000000000000000, -0.7421532822901560911 ) ) ;
#12099 = CARTESIAN_POINT ( 'NONE',  ( 2.913591648697507974, 17.99578554531247576, 8.387739717085498370 ) ) ;
#12101 = ORIENTED_EDGE ( 'NONE', *, *, #19262, .F. ) ;
#12102 = AXIS2_PLACEMENT_3D ( 'NONE', #7032, #18863, #734 ) ;
#12103 = DIRECTION ( 'NONE',  ( 0.000000000000000000, -1.000000000000000000, 0.000000000000000000 ) ) ;
#12104 = CARTESIAN_POINT ( 'NONE',  ( 6.013049556678311092, 11.37554327182399305, 2.937595415487594064 ) ) ;
#12105 = EDGE_CURVE ( 'NONE', #13712, #3547, #10381, .T. ) ;
#12106 = ADVANCED_FACE ( 'NONE', ( #713 ), #9334, .F. ) ;
#12107 = AXIS2_PLACEMENT_3D ( 'NONE', #11440, #21269, #3037 ) ;
#12108 = ORIENTED_EDGE ( 'NONE', *, *, #1311, .T. ) ;
#12109 = CARTESIAN_POINT ( 'NONE',  ( 8.607975884807220979, 19.62966740229102314, 6.049914683357609846 ) ) ;
#12110 = CARTESIAN_POINT ( 'NONE',  ( 10.70304827739237652, 21.11777521280046344, 0.2911716477774642930 ) ) ;
#12111 = CARTESIAN_POINT ( 'NONE',  ( 4.431163241856458157, 18.91035477026892409, -0.6033642490446163853 ) ) ;
#12112 = CARTESIAN_POINT ( 'NONE',  ( 11.29543655879299102, 22.16525292274814163, 2.036776594994900158 ) ) ;
#12113 = CARTESIAN_POINT ( 'NONE',  ( 21.03437500000000071, 32.54502000000000095, 5.159374999999999822 ) ) ;
#12114 = CIRCLE ( 'NONE', #14954, 0.5079999999999997851 ) ;
#12115 = CARTESIAN_POINT ( 'NONE',  ( 16.88793093518696509, 0.9484654469177136171, -15.18277371644746765 ) ) ;
#12116 = UNCERTAINTY_MEASURE_WITH_UNIT (LENGTH_MEASURE( 1.000000000000000082E-05 ), #10539, 'distance_accuracy_value', 'NONE');
#12117 = CARTESIAN_POINT ( 'NONE',  ( -4.728951812473551897, 28.56769750000000130, -29.02782796843600011 ) ) ;
#12118 = ORIENTED_EDGE ( 'NONE', *, *, #5034, .F. ) ;
#12119 = CARTESIAN_POINT ( 'NONE',  ( 11.21722422336513958, 15.53347034410194638, 6.755855952064321102 ) ) ;
#12120 = CARTESIAN_POINT ( 'NONE',  ( 9.486626320258515932, 19.32892518063468046, -2.981737702492698094 ) ) ;
#12121 = ORIENTED_EDGE ( 'NONE', *, *, #11278, .F. ) ;
#12122 = CARTESIAN_POINT ( 'NONE',  ( 10.60309855497350995, 11.60677215276931307, 3.485811182180083012 ) ) ;
#12123 = CARTESIAN_POINT ( 'NONE',  ( 66.87634738983680904, 0.000000000000000000, 3.497859541731999755 ) ) ;
#12124 = CARTESIAN_POINT ( 'NONE',  ( 12.84499073484238529, 22.15877926570874479, 0.4069147557942170979 ) ) ;
#12125 = CIRCLE ( 'NONE', #18117, 0.5079999999999996740 ) ;
#12127 = CARTESIAN_POINT ( 'NONE',  ( 12.91059077353605211, 21.25996874134203907, -21.27604296009081253 ) ) ;
#12126 = CARTESIAN_POINT ( 'NONE',  ( -0.4924320145162884854, 15.60814665309257343, 0.1703380108912158075 ) ) ;
#12128 = ORIENTED_EDGE ( 'NONE', *, *, #36, .F. ) ;
#12129 = CARTESIAN_POINT ( 'NONE',  ( 6.608070263590670734, 10.94537441895658247, 3.759284071021552265 ) ) ;
#12130 = DIRECTION ( 'NONE',  ( 0.2490110332224857170, 0.000000000000000000, -0.9685006480810790519 ) ) ;
#12131 = VERTEX_POINT ( 'NONE', #18279 ) ;
#12132 = EDGE_CURVE ( 'NONE', #15472, #6031, #16917, .T. ) ;
#12133 = CARTESIAN_POINT ( 'NONE',  ( 0.1546840198724105664, 13.50064022236746197, 1.919107787120799546 ) ) ;
#12134 = CIRCLE ( 'NONE', #2951, 0.7950200000000003930 ) ;
#12135 = EDGE_CURVE ( 'NONE', #3524, #1698, #6947, .T. ) ;
#12136 = FACE_BOUND ( 'NONE', #16640, .T. ) ;
#12137 = ORIENTED_EDGE ( 'NONE', *, *, #18200, .T. ) ;
#12138 = CARTESIAN_POINT ( 'NONE',  ( 13.36585934105912976, 21.37707621349031228, 1.842755075219712380 ) ) ;
#12139 = CARTESIAN_POINT ( 'NONE',  ( -5.863861779363051419, 34.12394749999999988, -34.80955303575778714 ) ) ;
#12140 = CARTESIAN_POINT ( 'NONE',  ( 55.27198911326564001, 34.52875999999999834, 2.462719476673013830 ) ) ;
#12141 = CARTESIAN_POINT ( 'NONE',  ( 5.396977437131427635, 17.85491577864669210, 8.577743016638430973 ) ) ;
#12142 = CARTESIAN_POINT ( 'NONE',  ( -12.30312499999999964, 2.380615000000000148, 8.731249999999999289 ) ) ;
#12143 = ORIENTED_EDGE ( 'NONE', *, *, #2239, .F. ) ;
#12144 = DIRECTION ( 'NONE',  ( 0.000000000000000000, 1.000000000000000000, 0.000000000000000000 ) ) ;
#12145 = CARTESIAN_POINT ( 'NONE',  ( 8.011380105705496746, 39.28205249999999893, -19.05252355006962617 ) ) ;
#12146 = LINE ( 'NONE', #13809, #9902 ) ;
#12147 = DIRECTION ( 'NONE',  ( -1.000000000000000000, 0.000000000000000000, 0.000000000000000000 ) ) ;
#12149 = CARTESIAN_POINT ( 'NONE',  ( 14.88133261977736232, -7.156567809876259290, -15.09667001033014166 ) ) ;
#12148 = DIRECTION ( 'NONE',  ( 0.000000000000000000, 1.000000000000000000, 0.000000000000000000 ) ) ;
#12150 = VECTOR ( 'NONE', #17135, 1000.000000000000000 ) ;
#12151 = ORIENTED_EDGE ( 'NONE', *, *, #83, .T. ) ;
#12152 = ORIENTED_EDGE ( 'NONE', *, *, #14024, .T. ) ;
#12153 = CARTESIAN_POINT ( 'NONE',  ( 5.580593771912873535, 15.56575848494070868, -1.427280786813629021 ) ) ;
#12154 = CARTESIAN_POINT ( 'NONE',  ( 1.272552473378664173, 21.11368951514764092, 3.304751149015114464 ) ) ;
#12155 = ORIENTED_EDGE ( 'NONE', *, *, #12357, .T. ) ;
#12156 = CARTESIAN_POINT ( 'NONE',  ( 5.336823734216668669, 12.43211864545296130, 7.110286411329449052 ) ) ;
#12157 = EDGE_LOOP ( 'NONE', ( #9356, #7934, #9920, #2763 ) ) ;
#12158 = VERTEX_POINT ( 'NONE', #9661 ) ;
#12159 = CIRCLE ( 'NONE', #11097, 0.3962400000000008138 ) ;
#12160 = CARTESIAN_POINT ( 'NONE',  ( 7.714989009133786269, 18.22557723514703909, -1.778184321832799064 ) ) ;
#12161 = EDGE_CURVE ( 'NONE', #13027, #10152, #10117, .T. ) ;
#12162 = ORIENTED_EDGE ( 'NONE', *, *, #1147, .F. ) ;
#12163 = CARTESIAN_POINT ( 'NONE',  ( 3.429843259907740638, 15.08894331730447824, 8.264066473586211714 ) ) ;
#12164 = AXIS2_PLACEMENT_3D ( 'NONE', #5896, #9212, #20944 ) ;
#12165 = FACE_OUTER_BOUND ( 'NONE', #18781, .T. ) ;
#12166 = FACE_OUTER_BOUND ( 'NONE', #21765, .T. ) ;
#12167 = CARTESIAN_POINT ( 'NONE',  ( 2.774532003195825158, 20.20761322045536801, 7.401467972215330704 ) ) ;
#12168 = LINE ( 'NONE', #17244, #13705 ) ;
#12169 = EDGE_LOOP ( 'NONE', ( #7364, #1541, #11054, #17876 ) ) ;
#12170 = CARTESIAN_POINT ( 'NONE',  ( 6.497001381719418767, 20.52421269917602231, 5.165954059377466656 ) ) ;
#12171 = VECTOR ( 'NONE', #18584, 1000.000000000000000 ) ;
#12172 = DIRECTION ( 'NONE',  ( 0.000000000000000000, 1.000000000000000000, 0.000000000000000000 ) ) ;
#12173 = CARTESIAN_POINT ( 'NONE',  ( 52.69120237754506064, -5.316777432816555127, -17.13598543997957080 ) ) ;
#12174 = DIRECTION ( 'NONE',  ( -0.2490110332224848011, 0.000000000000000000, 0.9685006480810792739 ) ) ;
#12175 = VERTEX_POINT ( 'NONE', #8000 ) ;
#12176 = CARTESIAN_POINT ( 'NONE',  ( 10.99454862271408118, 17.69506805168922980, 7.542432694877700072 ) ) ;
#12177 = CARTESIAN_POINT ( 'NONE',  ( 54.88544852023625253, 38.88803500000000213, -18.42785536490203668 ) ) ;
#12178 = CARTESIAN_POINT ( 'NONE',  ( 11.15535515337743355, 22.04911995710877193, 1.564565634628638291 ) ) ;
#12179 = VERTEX_POINT ( 'NONE', #13112 ) ;
#12180 = AXIS2_PLACEMENT_3D ( 'NONE', #323, #8497, #15279 ) ;
#12181 = ORIENTED_EDGE ( 'NONE', *, *, #4496, .F. ) ;
#12182 = CARTESIAN_POINT ( 'NONE',  ( 48.58367710892853353, 32.54502000000000095, -25.32442392637788231 ) ) ;
#12183 = CARTESIAN_POINT ( 'NONE',  ( 8.466430781601271605, 10.75601055456078292, 3.008801692261342531 ) ) ;
#12184 = CARTESIAN_POINT ( 'NONE',  ( 4.941667063029573370, 12.10288835339510172, 5.331384855635830533 ) ) ;
#12185 = FACE_OUTER_BOUND ( 'NONE', #12307, .T. ) ;
#12186 = CARTESIAN_POINT ( 'NONE',  ( 5.701223588767351025, 13.46368314359502172, -0.4004066624196506718 ) ) ;
#12187 = CARTESIAN_POINT ( 'NONE',  ( 7.259060271705660483, 16.62791818454387638, 7.622863755745528991 ) ) ;
#12188 = EDGE_CURVE ( 'NONE', #9189, #10775, #6236, .T. ) ;
#12189 = CARTESIAN_POINT ( 'NONE',  ( 39.00487391863466513, 40.07742955315917044, -3.894748490060887747 ) ) ;
#12190 = CARTESIAN_POINT ( 'NONE',  ( 8.731341498189751249, 21.27400681123072346, -0.2105259513614896327 ) ) ;
#12191 = CARTESIAN_POINT ( 'NONE',  ( 4.991580028654951207, 12.36007056541882676, 5.665111606981183101 ) ) ;
#12192 = AXIS2_PLACEMENT_3D ( 'NONE', #6606, #16682, #6930 ) ;
#12193 = CARTESIAN_POINT ( 'NONE',  ( 13.40968688455454405, 21.37908828663751848, 1.829925544955474104 ) ) ;
#12194 = CARTESIAN_POINT ( 'NONE',  ( 0.02568036181144206509, 12.52652910124526109, 1.670289039172707657 ) ) ;
#12195 = CARTESIAN_POINT ( 'NONE',  ( 1.145631384210077153, 19.30514743024435731, 8.620931369668081601 ) ) ;
#12196 = CARTESIAN_POINT ( 'NONE',  ( 19.87209107541814035, -0.1962630820641820817, -14.85150087166202226 ) ) ;
#12197 = CARTESIAN_POINT ( 'NONE',  ( 3.332789469297661622, 13.61441523003558274, 7.617045249923235950 ) ) ;
#12198 = DIRECTION ( 'NONE',  ( 0.000000000000000000, 1.000000000000000000, 0.000000000000000000 ) ) ;
#12199 = CYLINDRICAL_SURFACE ( 'NONE', #7964, 0.3962399999999999811 ) ;
#12200 = CARTESIAN_POINT ( 'NONE',  ( 13.04431081968415462, 1.431559631576304170, -16.33551417402710726 ) ) ;
#12201 = DIRECTION ( 'NONE',  ( 0.000000000000000000, -1.000000000000000000, 0.000000000000000000 ) ) ;
#12202 = CARTESIAN_POINT ( 'NONE',  ( 10.12849651354907188, 21.37172880332488134, 4.537220786037014619 ) ) ;
#12203 = EDGE_CURVE ( 'NONE', #18449, #6418, #7895, .T. ) ;
#12204 = LINE ( 'NONE', #20580, #3941 ) ;
#12205 = CARTESIAN_POINT ( 'NONE',  ( 11.74400045100115442, 11.53932207960275313, -0.3771188630170393963 ) ) ;
#12206 = CARTESIAN_POINT ( 'NONE',  ( 53.95242430215955665, 38.88803500000000213, -23.51676380836238067 ) ) ;
#12207 = ORIENTED_EDGE ( 'NONE', *, *, #691, .F. ) ;
#12208 = APPLICATION_PROTOCOL_DEFINITION ( 'draft international standard', 'automotive_design', 1998, #20604 ) ;
#12209 = AXIS2_PLACEMENT_3D ( 'NONE', #3903, #15193, #15310 ) ;
#12210 = CARTESIAN_POINT ( 'NONE',  ( 1.416441012474776606, -1.564831550500477730, -20.74814719358344917 ) ) ;
#12211 = EDGE_CURVE ( 'NONE', #1715, #3845, #7665, .T. ) ;
#12212 = EDGE_CURVE ( 'NONE', #3115, #4911, #16527, .T. ) ;
#12213 = EDGE_CURVE ( 'NONE', #10171, #9714, #9409, .T. ) ;
#12214 = LINE ( 'NONE', #10541, #2284 ) ;
#12215 = CARTESIAN_POINT ( 'NONE',  ( 21.61819370792156292, -3.402680683349632140, -15.07300270223215222 ) ) ;
#12216 = ORIENTED_EDGE ( 'NONE', *, *, #21352, .F. ) ;
#12217 = CARTESIAN_POINT ( 'NONE',  ( 10.78489084012707444, 11.65180524149912245, 3.851168386773756946 ) ) ;
#12218 = CARTESIAN_POINT ( 'NONE',  ( 4.732537519185278541, 19.32618335802288456, 6.876597588250359827 ) ) ;
#12219 = CARTESIAN_POINT ( 'NONE',  ( 6.423071385528279720, 20.04707047619034199, 0.2023860023504502892 ) ) ;
#12220 = CARTESIAN_POINT ( 'NONE',  ( 0.1034156370570294553, 15.60814665309257343, -0.008097649473000866072 ) ) ;
#12221 = DIRECTION ( 'NONE',  ( 0.2490110332224846346, 0.000000000000000000, -0.9685006480810792739 ) ) ;
#12222 = CARTESIAN_POINT ( 'NONE',  ( 18.72819589094305570, -0.2033655786179353053, -14.60285019604222967 ) ) ;
#12223 = CARTESIAN_POINT ( 'NONE',  ( 11.77608582838452023, -4.423560565762836738, -15.53037780770169363 ) ) ;
#12224 = ORIENTED_EDGE ( 'NONE', *, *, #2790, .F. ) ;
#12225 = CARTESIAN_POINT ( 'NONE',  ( 10.44704334393187040, 21.01241846032922211, 5.354331383626338869 ) ) ;
#12226 = EDGE_CURVE ( 'NONE', #9905, #17792, #21376, .T. ) ;
#12227 = EDGE_LOOP ( 'NONE', ( #631, #6933, #9692, #13030 ) ) ;
#12228 = CARTESIAN_POINT ( 'NONE',  ( 9.611418352984147262, 12.34090135786862064, -0.8804288050913021690 ) ) ;
#12229 = DIRECTION ( 'NONE',  ( -0.9790635044817342925, 0.000000000000000000, 0.2035550397114870846 ) ) ;
#12230 = DIRECTION ( 'NONE',  ( 0.000000000000000000, 1.000000000000000000, 0.000000000000000000 ) ) ;
#12231 = CARTESIAN_POINT ( 'NONE',  ( 7.200333630658113826, 16.63782405840064982, 8.499115931225610154 ) ) ;
#12232 = VERTEX_POINT ( 'NONE', #2707 ) ;
#12233 = CARTESIAN_POINT ( 'NONE',  ( 30.78626241496060700, 38.48766750000000059, -2.552201779827368622 ) ) ;
#12234 = ORIENTED_EDGE ( 'NONE', *, *, #5876, .F. ) ;
#12235 = ADVANCED_FACE ( 'NONE', ( #1259 ), #9863, .F. ) ;
#12236 = FACE_OUTER_BOUND ( 'NONE', #750, .T. ) ;
#12237 = CARTESIAN_POINT ( 'NONE',  ( 0.09157794466913266040, 16.58397131323004459, 0.8032362651113809093 ) ) ;
#12238 = CARTESIAN_POINT ( 'NONE',  ( 8.505511374756364873, 34.12394749999999988, -20.97439202360551747 ) ) ;
#12239 = ORIENTED_EDGE ( 'NONE', *, *, #3350, .F. ) ;
#12240 = CARTESIAN_POINT ( 'NONE',  ( 53.00421038040393995, 32.54502000000000095, 6.511420152579801446 ) ) ;
#12241 = AXIS2_PLACEMENT_3D ( 'NONE', #2324, #9058, #4432 ) ;
#12242 = CARTESIAN_POINT ( 'NONE',  ( 42.79471501377724252, 32.54502000000000095, 5.049205022181460834 ) ) ;
#12243 = LINE ( 'NONE', #6824, #2826 ) ;
#12244 = DIRECTION ( 'NONE',  ( 0.9636276526537417286, 0.000000000000000000, -0.2672484743474500268 ) ) ;
#12245 = CARTESIAN_POINT ( 'NONE',  ( 46.03750000000000142, 0.000000000000000000, -10.31874999999999964 ) ) ;
#12246 = ORIENTED_EDGE ( 'NONE', *, *, #16028, .T. ) ;
#12247 = DIRECTION ( 'NONE',  ( 0.000000000000000000, 1.000000000000000000, 0.000000000000000000 ) ) ;
#12248 = CARTESIAN_POINT ( 'NONE',  ( -13.87747867115857936, -3.968114999999999615, -9.458632424640695646 ) ) ;
#12249 = EDGE_CURVE ( 'NONE', #9499, #17581, #19303, .T. ) ;
#12250 = LINE ( 'NONE', #12479, #7729 ) ;
#12252 = CARTESIAN_POINT ( 'NONE',  ( 12.53020504515603761, -5.716024679458021396, -15.56730839992324356 ) ) ;
#12251 = DIRECTION ( 'NONE',  ( 1.000000000000000000, 0.000000000000000000, 0.000000000000000000 ) ) ;
#12253 = ORIENTED_EDGE ( 'NONE', *, *, #17748, .T. ) ;
#12254 = ADVANCED_FACE ( 'NONE', ( #11441 ), #13224, .F. ) ;
#12255 = EDGE_LOOP ( 'NONE', ( #5805, #20486, #16004, #3663, #21510 ) ) ;
#12256 = ADVANCED_FACE ( 'NONE', ( #11214 ), #19710, .F. ) ;
#12257 = CARTESIAN_POINT ( 'NONE',  ( 11.04394092023493279, 14.44257473674272241, -3.305683158826597356 ) ) ;
#12259 = FACE_OUTER_BOUND ( 'NONE', #15595, .T. ) ;
#12258 = CARTESIAN_POINT ( 'NONE',  ( 3.822081440817369558, 12.20035416735056266, 0.3768256591275319645 ) ) ;
#12260 = ORIENTED_EDGE ( 'NONE', *, *, #19488, .T. ) ;
#12262 = CARTESIAN_POINT ( 'NONE',  ( 20.32304652538368828, -6.633862778167403107, -14.99920447863399353 ) ) ;
#12261 = CARTESIAN_POINT ( 'NONE',  ( 5.600389116865858163, 15.22982981733899166, 8.688047065010637837 ) ) ;
#12263 = EDGE_LOOP ( 'NONE', ( #5096, #5054, #12587, #335 ) ) ;
#12264 = CIRCLE ( 'NONE', #13686, 9.524999999999996803 ) ;
#12265 = VERTEX_POINT ( 'NONE', #2814 ) ;
#12266 = CARTESIAN_POINT ( 'NONE',  ( 7.499759535020694479, 13.88337118655590707, -1.456658198050375663 ) ) ;
#12267 = ORIENTED_EDGE ( 'NONE', *, *, #7931, .F. ) ;
#12268 = DIRECTION ( 'NONE',  ( 0.000000000000000000, 1.000000000000000000, 0.000000000000000000 ) ) ;
#12269 = DIRECTION ( 'NONE',  ( 0.8583349619704310207, 0.000000000000000000, -0.5130897514657826175 ) ) ;
#12270 = PLANE ( 'NONE',  #11466 ) ;
#12271 = CARTESIAN_POINT ( 'NONE',  ( 3.541706160064697961, 17.13097328727698354, 9.143733616943571008 ) ) ;
#12272 = CARTESIAN_POINT ( 'NONE',  ( 17.79723720954694954, 36.51313500000000545, -14.07647485258271303 ) ) ;
#12273 = AXIS2_PLACEMENT_3D ( 'NONE', #6036, #16022, #7596 ) ;
#12274 = ORIENTED_EDGE ( 'NONE', *, *, #7459, .T. ) ;
#12275 = CARTESIAN_POINT ( 'NONE',  ( 2.845328762890635854, 20.46094657096126213, 6.331683592853763365 ) ) ;
#12276 = CARTESIAN_POINT ( 'NONE',  ( -29.36874999999999858, 30.56128000000000000, 8.731885000000000119 ) ) ;
#12277 = CARTESIAN_POINT ( 'NONE',  ( 12.99934549847542975, 21.71373124764409468, 2.001921367698964893 ) ) ;
#12278 = DIRECTION ( 'NONE',  ( 0.000000000000000000, 1.000000000000000000, 0.000000000000000000 ) ) ;
#12279 = ORIENTED_EDGE ( 'NONE', *, *, #1833, .T. ) ;
#12280 = ADVANCED_FACE ( 'NONE', ( #3038 ), #9762, .F. ) ;
#12281 = ORIENTED_EDGE ( 'NONE', *, *, #210, .T. ) ;
#12282 = CARTESIAN_POINT ( 'NONE',  ( 9.942270574732733124, 20.67808185030680335, 5.266683502927268279 ) ) ;
#12283 = CARTESIAN_POINT ( 'NONE',  ( 52.44708915697334106, -1.983739999999999837, 4.020247972991190188 ) ) ;
#12284 = CARTESIAN_POINT ( 'NONE',  ( 11.95009173601784269, 10.47212404987846135, 0.5522848250625118638 ) ) ;
#12285 = ORIENTED_EDGE ( 'NONE', *, *, #2073, .F. ) ;
#12286 = VERTEX_POINT ( 'NONE', #16632 ) ;
#12287 = CARTESIAN_POINT ( 'NONE',  ( 46.07940063401251507, 34.52875999999999834, -26.08707253294707229 ) ) ;
#12288 = CARTESIAN_POINT ( 'NONE',  ( 9.446499639003540949, 13.84869720761932577, 7.423493914728108933 ) ) ;
#12289 = CARTESIAN_POINT ( 'NONE',  ( 0.06378921647583885024, 14.29169281587572371, 1.241023057593835466 ) ) ;
#12290 = DIRECTION ( 'NONE',  ( 0.6702301885068638887, 0.000000000000000000, 0.7421532822901570903 ) ) ;
#12291 = CARTESIAN_POINT ( 'NONE',  ( 6.168663171305069248, 11.89819385903220095, 1.834497862875971164 ) ) ;
#12292 = CARTESIAN_POINT ( 'NONE',  ( 1.844819993078286480, 20.39307813490978560, 4.918341983821658658 ) ) ;
#12293 = CARTESIAN_POINT ( 'NONE',  ( -21.29909891687151813, -9.590920198756240467, -25.53841317587618320 ) ) ;
#12294 = CARTESIAN_POINT ( 'NONE',  ( 11.44565647860347823, 14.29921781272587289, -3.826291723331187722 ) ) ;
#12295 = CYLINDRICAL_SURFACE ( 'NONE', #17449, 0.5079999999999976756 ) ;
#12296 = CARTESIAN_POINT ( 'NONE',  ( -0.1939951092443372993, 13.90873432424026213, 0.5745305717807484003 ) ) ;
#12297 = CARTESIAN_POINT ( 'NONE',  ( -29.36874999999999858, 1.984375000000000000, -3.968750000000000000 ) ) ;
#12298 = CARTESIAN_POINT ( 'NONE',  ( 20.23296939222377233, -1.209661760518722762, -14.75693070578325106 ) ) ;
#12299 = CARTESIAN_POINT ( 'NONE',  ( 2.432517352912638486, 19.25811192615784151, 1.027623169201872688 ) ) ;
#12300 = CARTESIAN_POINT ( 'NONE',  ( 29.98909767165928386, 9.120187499999998337, -5.214162619065493054 ) ) ;
#12301 = CYLINDRICAL_SURFACE ( 'NONE', #12209, 0.3962399999999988154 ) ;
#12302 = CARTESIAN_POINT ( 'NONE',  ( 20.76278067970291374, -1.556605016331053637, -13.98716170710216211 ) ) ;
#12303 = DIRECTION ( 'NONE',  ( 0.2490110332224848289, 0.000000000000000000, -0.9685006480810792739 ) ) ;
#12304 = EDGE_CURVE ( 'NONE', #6777, #16794, #1475, .T. ) ;
#12305 = DIRECTION ( 'NONE',  ( 0.000000000000000000, 1.000000000000000000, 0.000000000000000000 ) ) ;
#12306 = CARTESIAN_POINT ( 'NONE',  ( 10.32709312739783059, 21.06472931975369889, 5.073596581982923404 ) ) ;
#12307 = EDGE_LOOP ( 'NONE', ( #14856, #6284, #11619, #20981 ) ) ;
#12308 = DIRECTION ( 'NONE',  ( 0.2490110332224850509, 0.000000000000000000, -0.9685006480810792739 ) ) ;
#12309 = CARTESIAN_POINT ( 'NONE',  ( 11.63972793865917943, 11.75705524565226057, -0.8376248640525733036 ) ) ;
#12310 = CARTESIAN_POINT ( 'NONE',  ( 14.39766489109863734, 1.100710950241990504, -15.99547158540225489 ) ) ;
#12311 = ORIENTED_EDGE ( 'NONE', *, *, #9141, .F. ) ;
#12312 = SHAPE_DEFINITION_REPRESENTATION ( #14096, #11018 ) ;
#12313 = CARTESIAN_POINT ( 'NONE',  ( 44.28293121686854761, 34.52875999999999834, -31.08068102505560759 ) ) ;
#12314 = ADVANCED_FACE ( 'NONE', ( #21712 ), #6566, .F. ) ;
#12315 = CARTESIAN_POINT ( 'NONE',  ( 2.063750000000000195, 1.984375000000000000, 8.335010000000000474 ) ) ;
#12316 = AXIS2_PLACEMENT_3D ( 'NONE', #15070, #3337, #9736 ) ;
#12317 = CARTESIAN_POINT ( 'NONE',  ( 20.48375339570359444, -0.2396799350905462478, -15.30716636276063447 ) ) ;
#12318 = EDGE_LOOP ( 'NONE', ( #11689, #12285, #7207, #2254 ) ) ;
#12319 = CARTESIAN_POINT ( 'NONE',  ( 12.56063288857526494, 19.93927778675710272, 5.046451759067746679 ) ) ;
#12320 = CARTESIAN_POINT ( 'NONE',  ( 7.562553572936893787, 21.00645437613600208, 3.186035226974327728 ) ) ;
#12321 = CARTESIAN_POINT ( 'NONE',  ( 2.907540519534558943, 11.61267145053902006, 3.383141968181686110 ) ) ;
#12322 = CARTESIAN_POINT ( 'NONE',  ( 51.69314645384351081, -6.356984999999999886, -17.03058447914853346 ) ) ;
#12323 = CYLINDRICAL_SURFACE ( 'NONE', #1562, 30.16249999999999076 ) ;
#12324 = AXIS2_PLACEMENT_3D ( 'NONE', #19595, #4461, #1132 ) ;
#12325 = CARTESIAN_POINT ( 'NONE',  ( 12.20717034251990540, -1.379848799635395640, -16.66392367771780414 ) ) ;
#12326 = UNCERTAINTY_MEASURE_WITH_UNIT (LENGTH_MEASURE( 1.000000000000000082E-05 ), #3461, 'distance_accuracy_value', 'NONE');
#12327 = DIRECTION ( 'NONE',  ( 0.000000000000000000, 1.000000000000000000, 0.000000000000000000 ) ) ;
#12328 = EDGE_CURVE ( 'NONE', #20613, #2429, #21810, .T. ) ;
#12329 = ORIENTED_EDGE ( 'NONE', *, *, #12105, .T. ) ;
#12330 = EDGE_CURVE ( 'NONE', #7937, #19449, #6500, .T. ) ;
#12331 = CARTESIAN_POINT ( 'NONE',  ( 6.500793124041273074, 10.79737175431668206, 3.223669991492981168 ) ) ;
#12332 = CARTESIAN_POINT ( 'NONE',  ( 39.11247911755811657, -5.166240873635326025, -4.078099790737317321 ) ) ;
#12333 = ORIENTED_EDGE ( 'NONE', *, *, #15387, .F. ) ;
#12334 = CARTESIAN_POINT ( 'NONE',  ( 9.294261281082977888, 15.43778034884425843, -2.770203070420261149 ) ) ;
#12335 = AXIS2_PLACEMENT_3D ( 'NONE', #18873, #8922, #12251 ) ;
#12336 = DIRECTION ( 'NONE',  ( 0.000000000000000000, 1.000000000000000000, 0.000000000000000000 ) ) ;
#12337 = DIRECTION ( 'NONE',  ( -0.2490110332224850509, 0.000000000000000000, 0.9685006480810792739 ) ) ;
#12339 = LINE ( 'NONE', #15787, #401 ) ;
#12338 = CARTESIAN_POINT ( 'NONE',  ( -0.4864308613666389891, 14.10021357005799025, 1.033949880137899680 ) ) ;
#12340 = ORIENTED_EDGE ( 'NONE', *, *, #15793, .F. ) ;
#12341 = CARTESIAN_POINT ( 'NONE',  ( 6.717861222798634735, 11.03073353602231066, 4.225789866886649371 ) ) ;
#12342 = CARTESIAN_POINT ( 'NONE',  ( 52.49113927203492125, -5.166360000000002728, -16.14695822742135078 ) ) ;
#12343 = AXIS2_PLACEMENT_3D ( 'NONE', #14915, #16663, #16773 ) ;
#12344 = VERTEX_POINT ( 'NONE', #20134 ) ;
#12345 = CARTESIAN_POINT ( 'NONE',  ( 12.79472653632228507, -3.968114999999999615, -13.31637763425449883 ) ) ;
#12346 = CARTESIAN_POINT ( 'NONE',  ( 0.03937504533965078407, 14.66358865000540668, 1.157625443383156760 ) ) ;
#12347 = AXIS2_PLACEMENT_3D ( 'NONE', #4888, #3450, #18367 ) ;
#12348 = CARTESIAN_POINT ( 'NONE',  ( 12.39411805528681576, -0.5459497824433883206, -16.72217961216554372 ) ) ;
#12349 = ORIENTED_EDGE ( 'NONE', *, *, #18262, .T. ) ;
#12350 = DIRECTION ( 'NONE',  ( -0.9964481331860212121, 0.000000000000000000, 0.08420877549337293932 ) ) ;
#12351 = CARTESIAN_POINT ( 'NONE',  ( 2.043921479127090102, 17.43725209588588143, 0.1880180425226697094 ) ) ;
#12352 = EDGE_CURVE ( 'NONE', #18598, #3856, #1795, .T. ) ;
#12353 = DIRECTION ( 'NONE',  ( 0.000000000000000000, 1.000000000000000000, 0.000000000000000000 ) ) ;
#12354 = CARTESIAN_POINT ( 'NONE',  ( 13.28822531734660828, -1.983739999999999393, -15.23578611614444078 ) ) ;
#12355 = DIRECTION ( 'NONE',  ( 0.2490110332224850509, 0.000000000000000000, -0.9685006480810792739 ) ) ;
#12356 = ORIENTED_EDGE ( 'NONE', *, *, #18913, .T. ) ;
#12357 = EDGE_CURVE ( 'NONE', #19608, #16034, #10836, .T. ) ;
#12358 = VECTOR ( 'NONE', #21120, 1000.000000000000227 ) ;
#12359 = CARTESIAN_POINT ( 'NONE',  ( 52.79771328282338771, 0.000000000000000000, 3.317700572842066986 ) ) ;
#12360 = DIRECTION ( 'NONE',  ( -0.000000000000000000, 1.000000000000000000, 0.000000000000000000 ) ) ;
#12361 = AXIS2_PLACEMENT_3D ( 'NONE', #20123, #794, #7541 ) ;
#12363 = CARTESIAN_POINT ( 'NONE',  ( 22.22454659879084460, -1.983739999999999393, -13.75904720189594244 ) ) ;
#12362 = PLANE ( 'NONE',  #4569 ) ;
#12364 = ORIENTED_EDGE ( 'NONE', *, *, #6140, .T. ) ;
#12365 = EDGE_LOOP ( 'NONE', ( #17978, #10574, #5887, #986 ) ) ;
#12366 = CARTESIAN_POINT ( 'NONE',  ( 5.630097896594783435, 13.98451010310800768, -0.8674368136027429399 ) ) ;
#12368 = FACE_OUTER_BOUND ( 'NONE', #12678, .T. ) ;
#12367 = CARTESIAN_POINT ( 'NONE',  ( 1.914114187929045308, 18.25211889560055667, -0.4709243356944546322 ) ) ;
#12369 = ORIENTED_EDGE ( 'NONE', *, *, #5007, .F. ) ;
#12371 = CARTESIAN_POINT ( 'NONE',  ( 20.06905745580504785, 0.5585409057930410537, -14.27919157916436532 ) ) ;
#12370 = CARTESIAN_POINT ( 'NONE',  ( 5.510631153008393568, 13.48046023248279113, 7.984051925542015482 ) ) ;
#12372 = ADVANCED_FACE ( 'NONE', ( #11871 ), #10095, .T. ) ;
#12373 = ORIENTED_EDGE ( 'NONE', *, *, #6584, .T. ) ;
#12374 = AXIS2_PLACEMENT_3D ( 'NONE', #20555, #19011, #2329 ) ;
#12375 = ORIENTED_EDGE ( 'NONE', *, *, #492, .T. ) ;
#12376 = CARTESIAN_POINT ( 'NONE',  ( 7.837419745790809245, 12.17652530823029622, 0.2379137956085111139 ) ) ;
#12377 = ORIENTED_EDGE ( 'NONE', *, *, #18142, .F. ) ;
#12378 = CIRCLE ( 'NONE', #352, 0.7950200000000000600 ) ;
#12379 = CARTESIAN_POINT ( 'NONE',  ( 2.997723901089916154, 12.34803938479561758, 5.822245433047846142 ) ) ;
#12380 = ADVANCED_FACE ( 'NONE', ( #15424 ), #1585, .T. ) ;
#12381 = ADVANCED_FACE ( 'NONE', ( #250 ), #6776, .T. ) ;
#12382 = EDGE_CURVE ( 'NONE', #19328, #395, #16943, .T. ) ;
#12383 = DIRECTION ( 'NONE',  ( -0.000000000000000000, -1.000000000000000000, 0.000000000000000000 ) ) ;
#12384 = DIRECTION ( 'NONE',  ( 0.1065921516619544457, 0.9937903127262237568, -0.03192064434796771516 ) ) ;
#12385 = DIRECTION ( 'NONE',  ( -0.2490110332224850509, 0.000000000000000000, 0.9685006480810792739 ) ) ;
#12386 = FACE_OUTER_BOUND ( 'NONE', #4639, .T. ) ;
#12387 = CARTESIAN_POINT ( 'NONE',  ( 1.476429774960471342, 21.14820369255740218, 3.937503551924574019 ) ) ;
#12388 = AXIS2_PLACEMENT_3D ( 'NONE', #13490, #21874, #18137 ) ;
#12389 = VERTEX_POINT ( 'NONE', #20460 ) ;
#12390 = CARTESIAN_POINT ( 'NONE',  ( 0.6684363650904089349, 20.56733048332889879, 6.164057930869264013 ) ) ;
#12391 = CARTESIAN_POINT ( 'NONE',  ( 12.79472653632228507, 34.52875999999999834, -13.31637763425449883 ) ) ;
#12392 = CARTESIAN_POINT ( 'NONE',  ( -0.8970842057359728061, 34.12394749999999988, -22.54358764576276286 ) ) ;
#12393 = CARTESIAN_POINT ( 'NONE',  ( 20.67155644328900621, -1.303699069785051456, -15.87085131396228199 ) ) ;
#12394 = ORIENTED_EDGE ( 'NONE', *, *, #14198, .T. ) ;
#12395 = VERTEX_POINT ( 'NONE', #6888 ) ;
#12396 = CARTESIAN_POINT ( 'NONE',  ( 9.067351539292140217, 12.06055924076114216, -1.205741145043526030 ) ) ;
#12397 = TOROIDAL_SURFACE ( 'NONE', #13451, 4.961572499999999941, 0.3962400000000000366 ) ;
#12398 = FACE_OUTER_BOUND ( 'NONE', #13836, .T. ) ;
#12399 = CARTESIAN_POINT ( 'NONE',  ( 13.35919779853531075, 14.07369424383953671, 6.735913025832823031 ) ) ;
#12400 = VERTEX_POINT ( 'NONE', #20349 ) ;
#12401 = VECTOR ( 'NONE', #16742, 1000.000000000000227 ) ;
#12402 = ORIENTED_EDGE ( 'NONE', *, *, #16504, .F. ) ;
#12403 = DIRECTION ( 'NONE',  ( -0.000000000000000000, -1.000000000000000000, 0.000000000000000000 ) ) ;
#12404 = CARTESIAN_POINT ( 'NONE',  ( 7.818102070580549068, 19.84329907872170651, -1.733884698244102518 ) ) ;
#12405 = CARTESIAN_POINT ( 'NONE',  ( 3.971545295231272643, 12.81903963674880131, 0.8759281729739175626 ) ) ;
#12406 = DIRECTION ( 'NONE',  ( 0.000000000000000000, -1.000000000000000000, -0.000000000000000000 ) ) ;
#12407 = CARTESIAN_POINT ( 'NONE',  ( 5.845438114022948994, 12.70542626881843695, 0.3374892689872108220 ) ) ;
#12408 = CIRCLE ( 'NONE', #7798, 1.983739999999999393 ) ;
#12409 = VECTOR ( 'NONE', #12539, 1000.000000000000000 ) ;
#12410 = CIRCLE ( 'NONE', #19778, 5.158739999999998105 ) ;
#12411 = CARTESIAN_POINT ( 'NONE',  ( 49.28028498622276032, -1.983739999999999837, -25.68670502218146368 ) ) ;
#12412 = EDGE_CURVE ( 'NONE', #13623, #10463, #17480, .T. ) ;
#12413 = CARTESIAN_POINT ( 'NONE',  ( 9.648314893053726138, 12.91190710784102080, 6.796865775111411878 ) ) ;
#12414 = PLANE ( 'NONE',  #18845 ) ;
#12415 = CARTESIAN_POINT ( 'NONE',  ( 5.606983389587787414, 15.64107961637180289, 8.866323357916209957 ) ) ;
#12416 = CARTESIAN_POINT ( 'NONE',  ( -0.1849527129589544072, 21.03045532914853055, 5.150944214860931680 ) ) ;
#12417 = DIRECTION ( 'NONE',  ( 0.9876802608827758290, 0.000000000000000000, -0.1564854698127972066 ) ) ;
#12418 = CARTESIAN_POINT ( 'NONE',  ( 5.025537597986745375, 20.64340025166658421, 2.222619301790576429 ) ) ;
#12419 = DIRECTION ( 'NONE',  ( -0.2868778675745011220, 0.000000000000000000, -0.9579671649362034858 ) ) ;
#12420 = DIRECTION ( 'NONE',  ( 0.000000000000000000, 1.000000000000000000, 0.000000000000000000 ) ) ;
#12421 = CARTESIAN_POINT ( 'NONE',  ( 20.96272718584998529, -3.045802774718411321, -13.88062344517622826 ) ) ;
#12422 = FACE_OUTER_BOUND ( 'NONE', #10451, .T. ) ;
#12423 = CIRCLE ( 'NONE', #11009, 1.190624999999997824 ) ;
#12424 = DIRECTION ( 'NONE',  ( 1.000000000000000000, 0.000000000000000000, 0.000000000000000000 ) ) ;
#12425 = CARTESIAN_POINT ( 'NONE',  ( 11.08308940409050081, 11.83732144666078590, 5.490605150716255878 ) ) ;
#12426 = ORIENTED_EDGE ( 'NONE', *, *, #1670, .T. ) ;
#12427 = DIRECTION ( 'NONE',  ( -0.000000000000000000, -1.000000000000000000, 0.000000000000000000 ) ) ;
#12428 = VECTOR ( 'NONE', #8295, 1000.000000000000000 ) ;
#12429 = CARTESIAN_POINT ( 'NONE',  ( 11.14440184571222048, 15.20245592030993542, -3.461858056394771399 ) ) ;
#12430 = CARTESIAN_POINT ( 'NONE',  ( 5.366014621799982010, 15.47125256599008480, -2.080610254137109649 ) ) ;
#12431 = FACE_OUTER_BOUND ( 'NONE', #20159, .T. ) ;
#12432 = CARTESIAN_POINT ( 'NONE',  ( 1.756216822573207104, 20.47856574081302128, 4.951414795929986568 ) ) ;
#12433 = ORIENTED_EDGE ( 'NONE', *, *, #4022, .T. ) ;
#12434 = PRODUCT_CONTEXT ( 'NONE', #8467, 'mechanical' ) ;
#12435 = SURFACE_STYLE_FILL_AREA ( #2131 ) ;
#12436 = CARTESIAN_POINT ( 'NONE',  ( 71.04062499999999147, 1.984375000000000000, -10.31874999999999964 ) ) ;
#12437 = AXIS2_PLACEMENT_3D ( 'NONE', #19322, #8939, #5620 ) ;
#12438 = EDGE_CURVE ( 'NONE', #17007, #17560, #18818, .T. ) ;
#12439 = VECTOR ( 'NONE', #17006, 1000.000000000000000 ) ;
#12440 = CARTESIAN_POINT ( 'NONE',  ( 10.38009686120726904, -3.119983079838188011, -17.18249216028544524 ) ) ;
#12441 = ORIENTED_EDGE ( 'NONE', *, *, #2518, .F. ) ;
#12442 = CARTESIAN_POINT ( 'NONE',  ( 8.205998663303592622, 20.59028652745482191, 4.708363946724399618 ) ) ;
#12443 = CARTESIAN_POINT ( 'NONE',  ( 5.638809941220587874, 13.98417111045325001, -0.8706810591892518714 ) ) ;
#12444 = CARTESIAN_POINT ( 'NONE',  ( 9.907371917564091746, -1.983739999999999393, -13.23786778167655243 ) ) ;
#12445 = VECTOR ( 'NONE', #18871, 1000.000000000000000 ) ;
#12446 = CIRCLE ( 'NONE', #14227, 1.785937499999999956 ) ;
#12447 = CARTESIAN_POINT ( 'NONE',  ( 20.09375723660039270, -1.415681770550045515, -14.79025032679060381 ) ) ;
#12448 = CARTESIAN_POINT ( 'NONE',  ( 16.22686663214561520, 1.074243784483314146, -15.38576787205390062 ) ) ;
#12449 = CARTESIAN_POINT ( 'NONE',  ( 20.23508736156870569, -1.359449706705495364, -14.75410053729980397 ) ) ;
#12450 = EDGE_CURVE ( 'NONE', #13109, #9688, #4131, .T. ) ;
#12451 = ORIENTED_EDGE ( 'NONE', *, *, #2047, .T. ) ;
#12452 = CARTESIAN_POINT ( 'NONE',  ( 11.14549571141843032, 18.39193805972417550, -4.149403309388357997 ) ) ;
#12453 = CARTESIAN_POINT ( 'NONE',  ( 54.11611804786240043, 30.56064500000000095, -30.58983753981140197 ) ) ;
#12454 = AXIS2_PLACEMENT_3D ( 'NONE', #7887, #21368, #6224 ) ;
#12455 = ORIENTED_EDGE ( 'NONE', *, *, #17236, .F. ) ;
#12456 = CARTESIAN_POINT ( 'NONE',  ( 9.381874342791970633, 16.98982907235301454, -2.824620680285168994 ) ) ;
#12457 = DIRECTION ( 'NONE',  ( 0.000000000000000000, 1.000000000000000000, 0.000000000000000000 ) ) ;
#12458 = DIRECTION ( 'NONE',  ( 1.000000000000000000, 0.000000000000000000, 0.000000000000000000 ) ) ;
#12460 = CARTESIAN_POINT ( 'NONE',  ( 29.19635173153840313, 32.54502000000000095, -6.218966092919240296 ) ) ;
#12459 = CARTESIAN_POINT ( 'NONE',  ( 4.947262131256387363, 17.41457342482845405, 8.526143230933524109 ) ) ;
#12461 = VERTEX_POINT ( 'NONE', #9279 ) ;
#12462 = CARTESIAN_POINT ( 'NONE',  ( 61.83151161312219557, 32.54502000000000095, -0.3645647634491749334 ) ) ;
#12463 = CIRCLE ( 'NONE', #2924, 0.3962399999999998701 ) ;
#12464 = CARTESIAN_POINT ( 'NONE',  ( 39.82184059222445427, -6.515279778729755833, -3.101326419564407910 ) ) ;
#12465 = VERTEX_POINT ( 'NONE', #1098 ) ;
#12466 = CARTESIAN_POINT ( 'NONE',  ( 19.37359715633457569, 0.4386801721828464951, -15.00800319500494950 ) ) ;
#12467 = ADVANCED_FACE ( 'NONE', ( #16157, #14496, #19235 ), #14618, .T. ) ;
#12468 = CARTESIAN_POINT ( 'NONE',  ( 20.17739840222535719, -1.548276265051773404, -15.86218595987928026 ) ) ;
#12469 = VERTEX_POINT ( 'NONE', #21325 ) ;
#12470 = CARTESIAN_POINT ( 'NONE',  ( 21.25660046192028929, -1.983739999999999393, -13.18703856829094079 ) ) ;
#12471 = CARTESIAN_POINT ( 'NONE',  ( 2.126660353523132319, 17.90725987158581134, 0.3359893863204973519 ) ) ;
#12472 = AXIS2_PLACEMENT_3D ( 'NONE', #16789, #1736, #8159 ) ;
#12473 = CARTESIAN_POINT ( 'NONE',  ( 13.18855152120810459, 18.81300736124048001, 6.748715921887202818 ) ) ;
#12474 = LINE ( 'NONE', #2051, #793 ) ;
#12475 = CARTESIAN_POINT ( 'NONE',  ( 46.03750000000000142, 34.52875999999999834, -10.31874999999999964 ) ) ;
#12476 = CIRCLE ( 'NONE', #21285, 1.190625000000000711 ) ;
#12477 = ORIENTED_EDGE ( 'NONE', *, *, #9543, .T. ) ;
#12478 = DIRECTION ( 'NONE',  ( 0.6744690509234938514, -0.7360996206939018904, -0.05699866455150646993 ) ) ;
#12479 = CARTESIAN_POINT ( 'NONE',  ( 49.41235866845560309, 30.56064500000000095, -26.78690084448080100 ) ) ;
#12481 = DIRECTION ( 'NONE',  ( -0.9579671649362032637, 0.000000000000000000, 0.2868778675745010664 ) ) ;
#12480 = DIRECTION ( 'NONE',  ( 0.000000000000000000, 1.000000000000000000, 0.000000000000000000 ) ) ;
#12482 = ORIENTED_EDGE ( 'NONE', *, *, #14796, .F. ) ;
#12483 = ORIENTED_EDGE ( 'NONE', *, *, #19071, .T. ) ;
#12484 = CARTESIAN_POINT ( 'NONE',  ( 0.7810342319177687731, 11.31615121391088152, 4.852052013636332539 ) ) ;
#12485 = ORIENTED_EDGE ( 'NONE', *, *, #21422, .F. ) ;
#12486 = CARTESIAN_POINT ( 'NONE',  ( 5.458294004585774850, 13.09016006394465670, 7.706839728735500827 ) ) ;
#12487 = ADVANCED_FACE ( 'NONE', ( #984 ), #11268, .T. ) ;
#12488 = ORIENTED_EDGE ( 'NONE', *, *, #8549, .T. ) ;
#12489 = ORIENTED_EDGE ( 'NONE', *, *, #14569, .T. ) ;
#12490 = EDGE_CURVE ( 'NONE', #4928, #7839, #2659, .T. ) ;
#12491 = VECTOR ( 'NONE', #11476, 1000.000000000000227 ) ;
#12492 = ORIENTED_EDGE ( 'NONE', *, *, #3670, .F. ) ;
#12493 = EDGE_CURVE ( 'NONE', #20833, #21044, #21104, .T. ) ;
#12494 = EDGE_CURVE ( 'NONE', #5923, #10689, #9162, .T. ) ;
#12495 = LINE ( 'NONE', #19219, #14580 ) ;
#12496 = VECTOR ( 'NONE', #10809, 1000.000000000000114 ) ;
#12497 = DIRECTION ( 'NONE',  ( -0.3542738219355896501, 0.000000000000000000, -0.9351417320872542627 ) ) ;
#12498 = CARTESIAN_POINT ( 'NONE',  ( 1.268730000000000135, 23.41816500000000190, 8.609509071587499562 ) ) ;
#12499 = PRODUCT_DEFINITION_SHAPE ( 'NONE', 'NONE',  #5596 ) ;
#12500 = DIRECTION ( 'NONE',  ( 0.000000000000000000, 1.000000000000000000, 0.000000000000000000 ) ) ;
#12501 = CARTESIAN_POINT ( 'NONE',  ( 2.418915203433949834, 20.78401357429190099, 6.470070638013244668 ) ) ;
#12502 = CARTESIAN_POINT ( 'NONE',  ( -6.100806958595617502, 34.12394749999684507, -35.21050882107662972 ) ) ;
#12503 = ORIENTED_EDGE ( 'NONE', *, *, #4566, .T. ) ;
#12504 = CARTESIAN_POINT ( 'NONE',  ( 4.881460237509400280, 11.69375961036644362, 3.716556164300745646 ) ) ;
#12505 = DIRECTION ( 'NONE',  ( 0.9685006480810787188, 0.000000000000000000, 0.2490110332224867162 ) ) ;
#12506 = DIRECTION ( 'NONE',  ( -0.9237641507921654505, 0.000000000000000000, -0.3829618697876189803 ) ) ;
#12507 = DIRECTION ( 'NONE',  ( -0.5087559856598098396, 0.000000000000000000, -0.8609107660235847392 ) ) ;
#12508 = DIRECTION ( 'NONE',  ( 1.000000000000000000, 0.000000000000000000, 0.000000000000000000 ) ) ;
#12509 = VERTEX_POINT ( 'NONE', #2875 ) ;
#12510 = CARTESIAN_POINT ( 'NONE',  ( 6.891132270267191551, 14.51543401643281150, -2.160190151449621787 ) ) ;
#12512 = CARTESIAN_POINT ( 'NONE',  ( 47.80475250345343596, 42.06303499999999929, -11.91473563638196786 ) ) ;
#12511 = CARTESIAN_POINT ( 'NONE',  ( 46.03750000000000142, 0.000000000000000000, -10.31874999999999964 ) ) ;
#12513 = AXIS2_PLACEMENT_3D ( 'NONE', #15904, #12575, #5477 ) ;
#12514 = CARTESIAN_POINT ( 'NONE',  ( 12.83058271130599692, 11.15713451920434096, 4.225958205527430067 ) ) ;
#12515 = ORIENTED_EDGE ( 'NONE', *, *, #316, .F. ) ;
#12516 = EDGE_CURVE ( 'NONE', #5609, #9456, #7735, .T. ) ;
#12517 = VERTEX_POINT ( 'NONE', #6071 ) ;
#12518 = DIRECTION ( 'NONE',  ( -0.9987059298363657467, 0.000000000000000000, -0.05085730733808409287 ) ) ;
#12519 = CARTESIAN_POINT ( 'NONE',  ( 7.300797866228468713, 13.50249100423538096, -2.124842999382142494 ) ) ;
#12520 = CARTESIAN_POINT ( 'NONE',  ( 2.532743019807210505, 12.01113885212942201, 3.567531869357724261 ) ) ;
#12521 = DIRECTION ( 'NONE',  ( 0.000000000000000000, 1.000000000000000000, 0.000000000000000000 ) ) ;
#12522 = CARTESIAN_POINT ( 'NONE',  ( 5.637115699025978088, 14.03407875391135207, -0.7791771547164595413 ) ) ;
#12523 = EDGE_CURVE ( 'NONE', #7062, #17451, #7627, .T. ) ;
#12524 = CYLINDRICAL_SURFACE ( 'NONE', #15327, 3.970020000000000326 ) ;
#12525 = CARTESIAN_POINT ( 'NONE',  ( 7.184449520472315776, 21.50782955549438213, 1.331064232565272398 ) ) ;
#12526 = CARTESIAN_POINT ( 'NONE',  ( 4.940276686280794749, 12.24160006483127106, 5.425643334560562359 ) ) ;
#12527 = VECTOR ( 'NONE', #16198, 1000.000000000000114 ) ;
#12528 = CARTESIAN_POINT ( 'NONE',  ( 21.25660046192028929, -3.968114999999999615, -13.18703856829094079 ) ) ;
#12529 = CARTESIAN_POINT ( 'NONE',  ( 7.115319024147658489, 11.65893940570930276, 6.012375857502059162 ) ) ;
#12530 = CARTESIAN_POINT ( 'NONE',  ( 1.585245561862221653, 17.17248089324893101, 9.542008508283084112 ) ) ;
#12531 = DIRECTION ( 'NONE',  ( -0.8609107660235848503, 0.000000000000000000, 0.5087559856598096175 ) ) ;
#12532 = CARTESIAN_POINT ( 'NONE',  ( 1.351641340660706847, 17.16051976808181578, 8.859800491581550475 ) ) ;
#12533 = FACE_OUTER_BOUND ( 'NONE', #12595, .T. ) ;
#12534 = CYLINDRICAL_SURFACE ( 'NONE', #17724, 0.7950200000000000600 ) ;
#12535 = CARTESIAN_POINT ( 'NONE',  ( 18.78053651718387229, 1.329081106205024954, -14.62912815047282855 ) ) ;
#12536 = AXIS2_PLACEMENT_3D ( 'NONE', #7454, #14112, #14228 ) ;
#12537 = VERTEX_POINT ( 'NONE', #21006 ) ;
#12538 = CARTESIAN_POINT ( 'NONE',  ( -16.07247711516169275, -2.588178535606159958, -10.44681224123558039 ) ) ;
#12539 = DIRECTION ( 'NONE',  ( 0.000000000000000000, 1.000000000000000000, 0.000000000000000000 ) ) ;
#12540 = CARTESIAN_POINT ( 'NONE',  ( 9.585720859379199155, 11.37056570364833163, -0.8501006578359496801 ) ) ;
#12541 = ORIENTED_EDGE ( 'NONE', *, *, #20170, .F. ) ;
#12542 = EDGE_CURVE ( 'NONE', #9016, #8141, #14740, .T. ) ;
#12543 = DIRECTION ( 'NONE',  ( -0.2490110332224846623, 0.000000000000000000, 0.9685006480810793850 ) ) ;
#12544 = EDGE_CURVE ( 'NONE', #2636, #12014, #1297, .T. ) ;
#12545 = CARTESIAN_POINT ( 'NONE',  ( 11.18523345132915736, 14.07407650860021775, -3.067769628887059064 ) ) ;
#12546 = CARTESIAN_POINT ( 'NONE',  ( 5.878563872623911557, 19.46939843988503682, -1.227892073574268217 ) ) ;
#12547 = LINE ( 'NONE', #7439, #11977 ) ;
#12548 = CARTESIAN_POINT ( 'NONE',  ( 2.108322636598648714, 12.53619568343860102, 2.181841141998187350 ) ) ;
#12549 = VERTEX_POINT ( 'NONE', #9495 ) ;
#12550 = DIRECTION ( 'NONE',  ( 0.2490110332224850509, 0.000000000000000000, -0.9685006480810792739 ) ) ;
#12551 = CARTESIAN_POINT ( 'NONE',  ( -5.863861779363051419, -1.594802499999999013, -34.80955303575778714 ) ) ;
#12552 = AXIS2_PLACEMENT_3D ( 'NONE', #10162, #18462, #1977 ) ;
#12553 = EDGE_LOOP ( 'NONE', ( #17911, #3753, #20461, #8257 ) ) ;
#12554 = CARTESIAN_POINT ( 'NONE',  ( 9.212431987401760836, 13.35013903698374094, 6.328237305530491241 ) ) ;
#12555 = FACE_OUTER_BOUND ( 'NONE', #2708, .T. ) ;
#12556 = CARTESIAN_POINT ( 'NONE',  ( 53.84486179190094646, -76.79125307200000350, -6.412645463410259872 ) ) ;
#12557 = DIRECTION ( 'NONE',  ( 0.000000000000000000, -1.000000000000000000, 0.000000000000000000 ) ) ;
#12558 = CARTESIAN_POINT ( 'NONE',  ( 4.490329389414642769, 20.73221372401878071, 6.369734200962422044 ) ) ;
#12559 = CARTESIAN_POINT ( 'NONE',  ( 14.58714708142341721, 0.8861103173364321961, -15.88890669882432682 ) ) ;
#12560 = CARTESIAN_POINT ( 'NONE',  ( -47.86049599909252805, 41.43438499999999891, -23.29373766372935961 ) ) ;
#12561 = ORIENTED_EDGE ( 'NONE', *, *, #14538, .T. ) ;
#12562 = CARTESIAN_POINT ( 'NONE',  ( 5.683261704384478641, 19.24102485395664175, -1.479744840059466826 ) ) ;
#12563 = CARTESIAN_POINT ( 'NONE',  ( 52.91086381164393515, 32.54502000000000095, 3.812938856729753301 ) ) ;
#12564 = AXIS2_PLACEMENT_3D ( 'NONE', #11153, #972, #4745 ) ;
#12565 = ORIENTED_EDGE ( 'NONE', *, *, #5849, .T. ) ;
#12566 = ADVANCED_FACE ( 'NONE', ( #5756 ), #16268, .T. ) ;
#12567 = CARTESIAN_POINT ( 'NONE',  ( 9.298577761259569030, 15.72771140787512856, -2.821255160405396811 ) ) ;
#12568 = CARTESIAN_POINT ( 'NONE',  ( -0.04547524747676359030, 20.22526626403869088, 5.510211994146467340 ) ) ;
#12570 = FACE_OUTER_BOUND ( 'NONE', #3599, .T. ) ;
#12569 = CARTESIAN_POINT ( 'NONE',  ( 0.3230198289976083381, 19.99706093811970220, 2.158794779438429234 ) ) ;
#12571 = ORIENTED_EDGE ( 'NONE', *, *, #15186, .T. ) ;
#12572 = DIRECTION ( 'NONE',  ( -1.000000000000000000, 0.000000000000000000, 0.000000000000000000 ) ) ;
#12573 = CARTESIAN_POINT ( 'NONE',  ( 39.18074928797054923, -7.516362886451771530, -3.705794944118392831 ) ) ;
#12574 = VERTEX_POINT ( 'NONE', #16373 ) ;
#12575 = DIRECTION ( 'NONE',  ( 1.000000000000000000, 0.000000000000000000, 0.000000000000000000 ) ) ;
#12576 = CARTESIAN_POINT ( 'NONE',  ( 0.06040298848788722835, 14.32294367124328538, 1.330604002369546013 ) ) ;
#12577 = CARTESIAN_POINT ( 'NONE',  ( 19.38085053746658915, -5.840261935552881312, -15.33262441706652268 ) ) ;
#12578 = EDGE_LOOP ( 'NONE', ( #7307, #20227, #12485, #19055 ) ) ;
#12579 = DIRECTION ( 'NONE',  ( -0.6702301885068628895, 0.000000000000000000, -0.7421532822901579785 ) ) ;
#12580 = CARTESIAN_POINT ( 'NONE',  ( 20.68769545271989330, -1.192153677757474384, -14.77120002427500900 ) ) ;
#12581 = CARTESIAN_POINT ( 'NONE',  ( 61.02111788801703085, 34.52875999999999834, -5.406220493519755088 ) ) ;
#12582 = CARTESIAN_POINT ( 'NONE',  ( 55.81697695389291169, -14.84248999999999974, -11.14520323105768362 ) ) ;
#12583 = VERTEX_POINT ( 'NONE', #2546 ) ;
#12584 = LINE ( 'NONE', #19202, #12856 ) ;
#12586 = CYLINDRICAL_SURFACE ( 'NONE', #12646, 15.47812499999999680 ) ;
#12585 = DIRECTION ( 'NONE',  ( 0.7421532822901580895, -0.000000000000000000, -0.6702301885068630005 ) ) ;
#12587 = ORIENTED_EDGE ( 'NONE', *, *, #18456, .F. ) ;
#12588 = VERTEX_POINT ( 'NONE', #20886 ) ;
#12589 = EDGE_CURVE ( 'NONE', #16799, #14245, #12954, .T. ) ;
#12590 = CARTESIAN_POINT ( 'NONE',  ( 5.376318597655482812, 12.35012481907357973, 7.177346072766759733 ) ) ;
#12591 = ORIENTED_EDGE ( 'NONE', *, *, #6160, .F. ) ;
#12592 = CARTESIAN_POINT ( 'NONE',  ( 4.758059951364139728, 11.14941623714734220, 4.549010102586493964 ) ) ;
#12593 = ORIENTED_EDGE ( 'NONE', *, *, #8232, .F. ) ;
#12594 = B_SPLINE_CURVE_WITH_KNOTS ( 'NONE', 3,
 ( #1783, #16832, #13642, #10422, #18588, #5540, #12298, #19026, #11966, #3455, #18918, #3678, #16, #8528, #17270, #1673, #17163, #20572, #8413, #351, #5210, #6883, #15189, #8742, #5431, #12196, #2116, #5113, #15308, #15641, #15523, #472, #6766, #20238, #16933, #131, #20342, #8644 ),
 .UNSPECIFIED., .F., .F.,
 ( 4, 2, 2, 2, 1, 1, 2, 2, 1, 2, 2, 2, 2, 1, 2, 2, 2, 2, 2, 1, 1, 4 ),
 ( 5.534983508193036528E-06, 0.04939775905433628489, 0.06174581507204322806, 0.06791984308089690781, 0.07409387108975057368, 0.09878998312516618086, 0.1234860951605817880, 0.1296601231694354261, 0.1358341511782890920, 0.1481822071959962572, 0.1975744312668257507, 0.2469666553376552443, 0.2593147113553626038, 0.2716627673730700465, 0.2963588794084849320, 0.3457511034793138704, 0.3704472155147284784, 0.3735342295191548811, 0.3750777365213670000, 0.3766212435235791745, 0.3827952715324290933, 0.3951433275501288200 ),
 .UNSPECIFIED. ) ;
#12595 = EDGE_LOOP ( 'NONE', ( #9040, #19911, #6660, #11409 ) ) ;
#12596 = VERTEX_POINT ( 'NONE', #17695 ) ;
#12597 = ADVANCED_FACE ( 'NONE', ( #16054 ), #10837, .T. ) ;
#12598 = CARTESIAN_POINT ( 'NONE',  ( 10.00557973814771984, 0.1597379260826150282, 9.514361097518639454 ) ) ;
#12599 = DIRECTION ( 'NONE',  ( -0.08420877549337300871, 0.000000000000000000, -0.9964481331860212121 ) ) ;
#12600 = DIRECTION ( 'NONE',  ( 0.000000000000000000, 1.000000000000000000, 0.000000000000000000 ) ) ;
#12601 = CARTESIAN_POINT ( 'NONE',  ( 3.546339648969794922, 13.37831192441575645, 8.288436347218903322 ) ) ;
#12602 = ORIENTED_EDGE ( 'NONE', *, *, #7315, .T. ) ;
#12603 = CARTESIAN_POINT ( 'NONE',  ( 2.000905577855156992, 14.11369167694475202, 8.640875553472284309 ) ) ;
#12604 = DIRECTION ( 'NONE',  ( -0.4128958666089269647, 0.5884034904305883718, 0.6951966166390366464 ) ) ;
#12605 = CARTESIAN_POINT ( 'NONE',  ( 0.2641497867371597752, 25.39269750000000059, -24.43980549416641068 ) ) ;
#12606 = CARTESIAN_POINT ( 'NONE',  ( 20.53156541068710439, -1.359447366214681985, -15.90722246059563361 ) ) ;
#12607 = VERTEX_POINT ( 'NONE', #14390 ) ;
#12608 = ORIENTED_EDGE ( 'NONE', *, *, #6603, .F. ) ;
#12609 = EDGE_CURVE ( 'NONE', #16794, #14138, #19643, .T. ) ;
#12610 = CARTESIAN_POINT ( 'NONE',  ( 6.490961022597671715, 21.20305659848830260, 1.632485957150709321 ) ) ;
#12611 = VECTOR ( 'NONE', #1039, 1000.000000000000000 ) ;
#12612 = ADVANCED_FACE ( 'NONE', ( #15946 ), #6726, .T. ) ;
#12614 = CARTESIAN_POINT ( 'NONE',  ( 59.74839655170352160, -6.356984999999999886, -15.51636860603746193 ) ) ;
#12613 = DIRECTION ( 'NONE',  ( 0.000000000000000000, 1.000000000000000000, 0.000000000000000000 ) ) ;
#12615 = CARTESIAN_POINT ( 'NONE',  ( 12.24639129257385761, 10.40896227699137100, 1.778670804891760771 ) ) ;
#12616 = ORIENTED_EDGE ( 'NONE', *, *, #20013, .T. ) ;
#12617 = ORIENTED_EDGE ( 'NONE', *, *, #14926, .F. ) ;
#12618 = CYLINDRICAL_SURFACE ( 'NONE', #10957, 1.190624999999997824 ) ;
#12619 = CARTESIAN_POINT ( 'NONE',  ( 7.847767795464331897, 11.20922263031854094, 0.3967533504084792551 ) ) ;
#12620 = LINE ( 'NONE', #7636, #4858 ) ;
#12621 = DIRECTION ( 'NONE',  ( 0.000000000000000000, 1.000000000000000000, 0.000000000000000000 ) ) ;
#12622 = B_SPLINE_CURVE_WITH_KNOTS ( 'NONE', 3,
 ( #15789, #21283, #7362, #20961, #19519, #14348, #20835, #726 ),
 .UNSPECIFIED., .F., .F.,
 ( 4, 2, 2, 4 ),
 ( 0.000000000000000000, 0.2499999999999988898, 0.4999999999999977796, 1.000000000000000000 ),
 .UNSPECIFIED. ) ;
#12623 = CARTESIAN_POINT ( 'NONE',  ( 6.371911847424065911, 19.85835382792685877, 0.1381288362860780827 ) ) ;
#12624 = CARTESIAN_POINT ( 'NONE',  ( 7.275815797620375669, 13.98176671473206056, 7.010075019451711853 ) ) ;
#12625 = LINE ( 'NONE', #6382, #1178 ) ;
#12626 = CARTESIAN_POINT ( 'NONE',  ( 29.36887348155339694, 30.56064500123875050, 10.71562877576799977 ) ) ;
#12627 = AXIS2_PLACEMENT_3D ( 'NONE', #6522, #16797, #1534 ) ;
#12628 = CARTESIAN_POINT ( 'NONE',  ( 9.179736842370099126, 21.96122921384184323, 1.647385027738300201 ) ) ;
#12629 = ADVANCED_FACE ( 'NONE', ( #13487 ), #7954, .T. ) ;
#12630 = CARTESIAN_POINT ( 'NONE',  ( 65.90927232300019512, -42.42568807200000691, -12.91110117861467899 ) ) ;
#12631 = CARTESIAN_POINT ( 'NONE',  ( -18.18961309330695997, 35.81157980123359863, -25.80119252674831998 ) ) ;
#12632 = CARTESIAN_POINT ( 'NONE',  ( 57.69402548289047417, 34.52875999999999834, -20.84562559047711261 ) ) ;
#12633 = CARTESIAN_POINT ( 'NONE',  ( 5.849665999842254216, 11.58475123937168050, 0.6023921236097111720 ) ) ;
#12634 = CARTESIAN_POINT ( 'NONE',  ( 22.04181838752732148, 16.26393749999999727, 0.06645525512612464325 ) ) ;
#12635 = DIRECTION ( 'NONE',  ( -0.3140771401027084853, 0.9459569826691583971, -0.08075231887918268847 ) ) ;
#12636 = CARTESIAN_POINT ( 'NONE',  ( -0.006835114654918546251, 15.70524387060945948, 0.7726394593941875444 ) ) ;
#12637 = PLANE ( 'NONE',  #14866 ) ;
#12638 = CARTESIAN_POINT ( 'NONE',  ( 44.27024749654614055, -6.356984999999999886, -8.722764363618502159 ) ) ;
#12639 = CARTESIAN_POINT ( 'NONE',  ( 18.28386440432367621, 1.638836122736962331, -14.77887936977548300 ) ) ;
#12640 = ORIENTED_EDGE ( 'NONE', *, *, #17426, .T. ) ;
#12641 = LINE ( 'NONE', #2573, #3237 ) ;
#12642 = EDGE_CURVE ( 'NONE', #10833, #13806, #11599, .T. ) ;
#12643 = CARTESIAN_POINT ( 'NONE',  ( 9.882996518030738642, 10.80489496159325213, 0.4162864141824605402 ) ) ;
#12644 = ORIENTED_EDGE ( 'NONE', *, *, #3397, .T. ) ;
#12645 = CARTESIAN_POINT ( 'NONE',  ( 25.20528082976425210, 1.004445366757521940, 10.45732921704471963 ) ) ;
#12646 = AXIS2_PLACEMENT_3D ( 'NONE', #21182, #17448, #2407 ) ;
#12647 = CARTESIAN_POINT ( 'NONE',  ( 28.38195592936287781, 29.75832250000000201, -13.81504834214261024 ) ) ;
#12648 = VERTEX_POINT ( 'NONE', #3317 ) ;
#12649 = CONTEXT_DEPENDENT_SHAPE_REPRESENTATION ( #2112, #18679 ) ;
#12650 = PLANE ( 'NONE',  #2127 ) ;
#12651 = CARTESIAN_POINT ( 'NONE',  ( -29.36874999999999858, 30.56064500000000095, 8.731249999999999289 ) ) ;
#12652 = EDGE_LOOP ( 'NONE', ( #13173, #9998, #10734, #1531, #7869 ) ) ;
#12653 = CARTESIAN_POINT ( 'NONE',  ( 10.38767455379903737, 20.34020649082646059, 4.891963057538385229 ) ) ;
#12654 = ADVANCED_FACE ( 'NONE', ( #20089 ), #8058, .F. ) ;
#12655 = CARTESIAN_POINT ( 'NONE',  ( 10.32478362973197861, 20.34432016293438039, 4.913735014817459223 ) ) ;
#12656 = CARTESIAN_POINT ( 'NONE',  ( 2.391149987034691282, 11.90891113418242142, 1.713267630547372855 ) ) ;
#12657 = EDGE_CURVE ( 'NONE', #17060, #17408, #15797, .T. ) ;
#12658 = CARTESIAN_POINT ( 'NONE',  ( -12.61651652020322523, -1.983740000000001613, -1.064728033956553244 ) ) ;
#12659 = EDGE_CURVE ( 'NONE', #17060, #8133, #2726, .T. ) ;
#12660 = CARTESIAN_POINT ( 'NONE',  ( 53.63200503474948277, -7.328454906157151783, -16.06800900404986265 ) ) ;
#12661 = CARTESIAN_POINT ( 'NONE',  ( 5.477890856393674568, 17.26865818392792562, 8.717832788898684626 ) ) ;
#12662 = CARTESIAN_POINT ( 'NONE',  ( 29.64606458365116737, -6.752907499999998286, -15.53894806404596096 ) ) ;
#12663 = ORIENTED_EDGE ( 'NONE', *, *, #18070, .F. ) ;
#12664 = PRODUCT_DEFINITION_FORMATION_WITH_SPECIFIED_SOURCE ( 'ANY', '', #9124, .NOT_KNOWN. ) ;
#12665 = CARTESIAN_POINT ( 'NONE',  ( 14.59864429982308032, -8.662966625467099391, -15.22137380051930045 ) ) ;
#12666 = CARTESIAN_POINT ( 'NONE',  ( 38.94885947252404179, -5.166721542084396823, -3.956611957468594287 ) ) ;
#12667 = EDGE_LOOP ( 'NONE', ( #1490, #1367, #16084, #20304 ) ) ;
#12668 = CARTESIAN_POINT ( 'NONE',  ( 10.06365592863438962, 20.01297154863687311, -1.326460872188967022 ) ) ;
#12669 = DIRECTION ( 'NONE',  ( 0.000000000000000000, 1.000000000000000000, 0.000000000000000000 ) ) ;
#12670 = CARTESIAN_POINT ( 'NONE',  ( 54.11611804786240043, 32.54502000000000095, -30.58983753981140197 ) ) ;
#12672 = CARTESIAN_POINT ( 'NONE',  ( -29.36874999999999858, 32.54502000000000095, 8.731885000000000119 ) ) ;
#12671 = CARTESIAN_POINT ( 'NONE',  ( -0.3012801303904104055, 12.83134191367328292, 2.046756627941362261 ) ) ;
#12673 = EDGE_LOOP ( 'NONE', ( #3421, #13325, #7957 ) ) ;
#12674 =( LENGTH_UNIT ( ) NAMED_UNIT ( * ) SI_UNIT ( .MILLI., .METRE. ) );
#12675 = LINE ( 'NONE', #20960, #9904 ) ;
#12676 = CARTESIAN_POINT ( 'NONE',  ( 30.78626241496060700, 1.982787499999999481, -2.552201779827368622 ) ) ;
#12677 = CIRCLE ( 'NONE', #8762, 3.968750000000000000 ) ;
#12678 = EDGE_LOOP ( 'NONE', ( #2398, #2274, #10225, #2198 ) ) ;
#12679 = DIRECTION ( 'NONE',  ( 0.000000000000000000, 1.000000000000000000, 0.000000000000000000 ) ) ;
#12680 = CARTESIAN_POINT ( 'NONE',  ( 11.66912023571120827, -3.656888143346838316, -15.82494830968131438 ) ) ;
#12681 = VERTEX_POINT ( 'NONE', #10151 ) ;
#12682 = CARTESIAN_POINT ( 'NONE',  ( 50.99913033092320092, 0.000000000000000000, -7.029081061492260751 ) ) ;
#12683 = VECTOR ( 'NONE', #3912, 1000.000000000000000 ) ;
#12684 = EDGE_CURVE ( 'NONE', #1375, #4259, #16587, .T. ) ;
#12685 = CARTESIAN_POINT ( 'NONE',  ( 11.21692919964015545, 18.39344551543875284, -4.174985455970938730 ) ) ;
#12686 = LINE ( 'NONE', #4281, #3799 ) ;
#12687 = VECTOR ( 'NONE', #9384, 1000.000000000000000 ) ;
#12688 = VERTEX_POINT ( 'NONE', #1424 ) ;
#12689 = DIRECTION ( 'NONE',  ( -0.3542738219355860418, 0.000000000000000000, -0.9351417320872557060 ) ) ;
#12690 = FACE_OUTER_BOUND ( 'NONE', #432, .T. ) ;
#12691 = ORIENTED_EDGE ( 'NONE', *, *, #16959, .F. ) ;
#12692 = ORIENTED_EDGE ( 'NONE', *, *, #15112, .F. ) ;
#12693 = CARTESIAN_POINT ( 'NONE',  ( 17.27120983696573120, 2.432768651782924785, -15.04950751273090148 ) ) ;
#12695 = DIRECTION ( 'NONE',  ( 0.9964481331860212121, 0.000000000000000000, -0.08420877549337300871 ) ) ;
#12694 = CARTESIAN_POINT ( 'NONE',  ( 7.591324994831230022, 14.71783044265311702, 8.261316382108162770 ) ) ;
#12696 = VERTEX_POINT ( 'NONE', #15150 ) ;
#12697 = CARTESIAN_POINT ( 'NONE',  ( 4.013474518967609761, 11.67735946699760241, 1.345522051684508336 ) ) ;
#12698 = AXIS2_PLACEMENT_3D ( 'NONE', #9843, #21574, #3018 ) ;
#12699 = ORIENTED_EDGE ( 'NONE', *, *, #11698, .T. ) ;
#12700 = ORIENTED_EDGE ( 'NONE', *, *, #17880, .F. ) ;
#12701 = ORIENTED_EDGE ( 'NONE', *, *, #8955, .T. ) ;
#12702 = CARTESIAN_POINT ( 'NONE',  ( 3.036164854790453393, 12.43340785568576301, 6.003854425968038200 ) ) ;
#12703 = EDGE_CURVE ( 'NONE', #21216, #1117, #21659, .T. ) ;
#12704 = VECTOR ( 'NONE', #17713, 1000.000000000000000 ) ;
#12705 = LINE ( 'NONE', #2422, #9957 ) ;
#12706 = AXIS2_PLACEMENT_3D ( 'NONE', #10268, #3206, #18459 ) ;
#12707 = CARTESIAN_POINT ( 'NONE',  ( 39.93069333242032570, 38.88803500000010160, -3.008993689095761148 ) ) ;
#12708 = LINE ( 'NONE', #2860, #10750 ) ;
#12709 = CARTESIAN_POINT ( 'NONE',  ( 13.67756757867809725, 38.48766750000000059, 2.571257636385987144 ) ) ;
#12710 = CARTESIAN_POINT ( 'NONE',  ( 2.181336132775622438, 11.71815103926796198, 2.193647000044615325 ) ) ;
#12711 = ORIENTED_EDGE ( 'NONE', *, *, #11625, .F. ) ;
#12712 = FACE_OUTER_BOUND ( 'NONE', #5819, .T. ) ;
#12713 = CARTESIAN_POINT ( 'NONE',  ( 9.058884679750676128, -1.983739999999999393, -16.32319115207028659 ) ) ;
#12714 = CARTESIAN_POINT ( 'NONE',  ( 13.05797387958584821, 21.99054487380438871, 2.024989902501916905 ) ) ;
#12715 = CARTESIAN_POINT ( 'NONE',  ( 10.10534066920194185, -1.983739999999999393, -14.00784516691476966 ) ) ;
#12716 = ORIENTED_EDGE ( 'NONE', *, *, #10097, .T. ) ;
#12717 = EDGE_LOOP ( 'NONE', ( #1823, #859, #13337, #9694 ) ) ;
#12718 = CARTESIAN_POINT ( 'NONE',  ( 8.988283004004445687, 14.76305577989238138, 7.604544232459095277 ) ) ;
#12719 = TOROIDAL_SURFACE ( 'NONE', #9866, 3.174999999999999822, 1.190625000000000044 ) ;
#12720 = APPLICATION_CONTEXT ( 'automotive_design' ) ;
#12722 = LINE ( 'NONE', #21326, #14566 ) ;
#12721 = DIRECTION ( 'NONE',  ( -0.6702301885068628895, 0.000000000000000000, -0.7421532822901579785 ) ) ;
#12723 = CARTESIAN_POINT ( 'NONE',  ( 13.37108644572652771, 14.27456381540390673, 6.816450116726900710 ) ) ;
#12724 = ORIENTED_EDGE ( 'NONE', *, *, #20453, .F. ) ;
#12725 = ORIENTED_EDGE ( 'NONE', *, *, #5838, .F. ) ;
#12726 = PLANE ( 'NONE',  #3207 ) ;
#12727 = CARTESIAN_POINT ( 'NONE',  ( 7.447520878388439236, 12.50167464702338194, -1.386640270854869961 ) ) ;
#12728 = CARTESIAN_POINT ( 'NONE',  ( 5.229630846777064690, 12.95116610613770369, 6.655177510049234968 ) ) ;
#12729 = AXIS2_PLACEMENT_3D ( 'NONE', #11639, #20344, #5320 ) ;
#12730 = VECTOR ( 'NONE', #17298, 1000.000000000000114 ) ;
#12731 = CARTESIAN_POINT ( 'NONE',  ( 6.405688018049387367, 19.93193575971154274, 0.2230809831250722963 ) ) ;
#12732 = CARTESIAN_POINT ( 'NONE',  ( 7.232330221986995156, 13.58629969230393186, 6.749857871587612301 ) ) ;
#12733 = CIRCLE ( 'NONE', #20071, 1.190624999999997824 ) ;
#12734 = CARTESIAN_POINT ( 'NONE',  ( 2.314778814167119059, 20.07314846742249514, 6.131468401820635350 ) ) ;
#12735 = CARTESIAN_POINT ( 'NONE',  ( 14.43917063414567536, -5.959792500000001603, 2.343183994106907697 ) ) ;
#12736 = ADVANCED_FACE ( 'NONE', ( #5074 ), #8166, .F. ) ;
#12737 = PRESENTATION_LAYER_ASSIGNMENT (  '', '', ( #15567 ) ) ;
#12738 = CARTESIAN_POINT ( 'NONE',  ( 5.864062336726267866, 19.24102485395664175, -1.533888344931878311 ) ) ;
#12739 = EDGE_CURVE ( 'NONE', #10568, #12990, #7676, .T. ) ;
#12740 = CARTESIAN_POINT ( 'NONE',  ( 13.54865253201757724, 22.13033908681270390, 1.898565167770253970 ) ) ;
#12741 = LINE ( 'NONE', #19021, #7561 ) ;
#12742 = FACE_OUTER_BOUND ( 'NONE', #11601, .T. ) ;
#12743 = CARTESIAN_POINT ( 'NONE',  ( -0.2458537890374220825, 15.59650202059448354, 0.006824066329813496118 ) ) ;
#12744 = CARTESIAN_POINT ( 'NONE',  ( 1.649085185276372156, 13.89508689931360763, 8.979946004438978946 ) ) ;
#12745 = CARTESIAN_POINT ( 'NONE',  ( 39.58386072796507449, 37.69740999999999786, -4.490541772578644064 ) ) ;
#12746 = AXIS2_PLACEMENT_3D ( 'NONE', #9576, #1184, #7926 ) ;
#12747 = CARTESIAN_POINT ( 'NONE',  ( 4.556409632327232728, 11.78043576488526156, 3.812351442791019451 ) ) ;
#12748 = CARTESIAN_POINT ( 'NONE',  ( 53.09667693522772680, 40.07859983757830946, -16.71356960103740619 ) ) ;
#12749 = LINE ( 'NONE', #4227, #16993 ) ;
#12750 = CARTESIAN_POINT ( 'NONE',  ( 12.40265734679424092, -7.252961835381453781, -15.64046151589976930 ) ) ;
#12751 = AXIS2_PLACEMENT_3D ( 'NONE', #8218, #14875, #17961 ) ;
#12752 = ORIENTED_EDGE ( 'NONE', *, *, #19487, .T. ) ;
#12753 = FACE_OUTER_BOUND ( 'NONE', #7166, .T. ) ;
#12754 = CARTESIAN_POINT ( 'NONE',  ( 10.44642686154466382, 10.62307989687129961, 2.768800612658094629 ) ) ;
#12755 = ORIENTED_EDGE ( 'NONE', *, *, #14813, .T. ) ;
#12756 = VECTOR ( 'NONE', #17550, 1000.000000000000000 ) ;
#12757 = CARTESIAN_POINT ( 'NONE',  ( 21.23834649789565177, 0.6614900943270459743, 10.21122617957944101 ) ) ;
#12758 = CARTESIAN_POINT ( 'NONE',  ( 12.38484231126942703, 20.96008087765395089, -0.8145651279088295116 ) ) ;
#12759 = VECTOR ( 'NONE', #19241, 1000.000000000000000 ) ;
#12760 = CARTESIAN_POINT ( 'NONE',  ( 5.365919581558607376, 15.46343705278112779, -2.079313974049490810 ) ) ;
#12761 = DIRECTION ( 'NONE',  ( 0.000000000000000000, 0.000000000000000000, 1.000000000000000000 ) ) ;
#12762 = CIRCLE ( 'NONE', #8495, 20.83593750000000000 ) ;
#12763 = ORIENTED_EDGE ( 'NONE', *, *, #12544, .F. ) ;
#12764 = EDGE_CURVE ( 'NONE', #13849, #7932, #21542, .T. ) ;
#12765 = FACE_OUTER_BOUND ( 'NONE', #5302, .T. ) ;
#12766 = CARTESIAN_POINT ( 'NONE',  ( 5.315554667604303951, 20.70596588439894603, 2.913411620298497873 ) ) ;
#12767 = CARTESIAN_POINT ( 'NONE',  ( 52.79771328282338771, 34.52875999999999834, 3.317700572842066986 ) ) ;
#12768 = EDGE_CURVE ( 'NONE', #16034, #2599, #18336, .T. ) ;
#12769 = ORIENTED_EDGE ( 'NONE', *, *, #9353, .T. ) ;
#12770 = CARTESIAN_POINT ( 'NONE',  ( 10.19446762859863753, 11.43307009487834058, 0.3353791086218075312 ) ) ;
#12771 = EDGE_CURVE ( 'NONE', #18859, #20415, #1649, .T. ) ;
#12772 = AXIS2_PLACEMENT_3D ( 'NONE', #4240, #21139, #2584 ) ;
#12773 = CARTESIAN_POINT ( 'NONE',  ( 9.325258829846921671, 14.88009260821627500, 7.099533925557936165 ) ) ;
#12774 = CARTESIAN_POINT ( 'NONE',  ( 46.03750000000000142, -3.968114999999999615, -10.31874999999999964 ) ) ;
#12775 = AXIS2_PLACEMENT_3D ( 'NONE', #21059, #7790, #10685 ) ;
#12776 = CARTESIAN_POINT ( 'NONE',  ( 53.83496721834958976, -6.979221732790449551, -15.78953645305750442 ) ) ;
#12777 = CARTESIAN_POINT ( 'NONE',  ( 20.39032348261012118, -1.415670249624013666, -15.94372942033169593 ) ) ;
#12778 = CARTESIAN_POINT ( 'NONE',  ( 5.128092007265404817, 19.14636313803755385, 7.990005468057869820 ) ) ;
#12779 = DIRECTION ( 'NONE',  ( 0.000000000000000000, 0.000000000000000000, -1.000000000000000000 ) ) ;
#12780 = CIRCLE ( 'NONE', #11362, 0.7950199999999993938 ) ;
#12781 = ORIENTED_EDGE ( 'NONE', *, *, #6085, .F. ) ;
#12782 = CARTESIAN_POINT ( 'NONE',  ( 8.011380105705496746, -6.752907499999998286, -19.05252355006962617 ) ) ;
#12783 = CARTESIAN_POINT ( 'NONE',  ( 10.66005185129409938, -4.911957254796272210, -16.03335128564671308 ) ) ;
#12784 = VECTOR ( 'NONE', #84, 1000.000000000000000 ) ;
#12785 = ORIENTED_EDGE ( 'NONE', *, *, #665, .F. ) ;
#12786 = CARTESIAN_POINT ( 'NONE',  ( 9.643460259527261158, 18.64508862159060598, -2.339718049086865204 ) ) ;
#12787 = CARTESIAN_POINT ( 'NONE',  ( 1.581041518826207248, -3.968114999999999615, -20.30277549736237575 ) ) ;
#12788 = CARTESIAN_POINT ( 'NONE',  ( 1.395580270598014927, 16.74552131709351954, 8.831485484237404648 ) ) ;
#12789 = CARTESIAN_POINT ( 'NONE',  ( 10.40440438601274487, -3.118828651999451473, -16.72929749093172092 ) ) ;
#12791 = CARTESIAN_POINT ( 'NONE',  ( 30.42699695299585017, 34.52875999999999834, -4.832012189960551041 ) ) ;
#12790 = CARTESIAN_POINT ( 'NONE',  ( 1.158249747892080794, 14.11369167694475202, 8.893221684370338664 ) ) ;
#12792 = ORIENTED_EDGE ( 'NONE', *, *, #20360, .F. ) ;
#12793 = ADVANCED_FACE ( 'NONE', ( #4641 ), #17612, .T. ) ;
#12794 = LINE ( 'NONE', #19517, #10647 ) ;
#12795 = CLOSED_SHELL ( 'NONE', ( #18839, #762, #9475, #10731, #15921, #2842, #20729, #19231, #12380, #15515, #20571, #15464, #4244, #21524, #21552, #1537, #6882, #7105, #17759, #18220, #21371, #16167, #21379, #5995, #16134, #15513, #9194, #15136, #21579, #20869, #11457, #3860, #1290, #12943, #16000, #15871, #167, #10468, #15627, #5197, #14946, #8896, #19880, #3747, #10548, #5974, #17755, #17462, #17700, #1336, #8463, #8693, #3866, #7056, #5656, #4980 ) ) ;
#12796 = CARTESIAN_POINT ( 'NONE',  ( 24.99127163628573456, 8.724202693596797786, 2.964528152719008158 ) ) ;
#12797 = AXIS2_PLACEMENT_3D ( 'NONE', #6072, #7526, #4433 ) ;
#12798 = EDGE_LOOP ( 'NONE', ( #7280, #7784 ) ) ;
#12799 = CARTESIAN_POINT ( 'NONE',  ( 20.04236263901815462, -1.092632170845033057, -14.81078003435047563 ) ) ;
#12800 = TOROIDAL_SURFACE ( 'NONE', #17017, 3.174999999999999822, 0.5953125000000000222 ) ;
#12801 = FACE_OUTER_BOUND ( 'NONE', #21100, .T. ) ;
#12802 = ORIENTED_EDGE ( 'NONE', *, *, #2791, .T. ) ;
#12803 = VECTOR ( 'NONE', #1985, 1000.000000000000000 ) ;
#12804 = CARTESIAN_POINT ( 'NONE',  ( 11.21434600409958549, 15.74974973885002250, 6.894954303353790337 ) ) ;
#12805 = CIRCLE ( 'NONE', #10302, 16.66874999999998508 ) ;
#12806 = DIRECTION ( 'NONE',  ( -0.9784543669157824697, 0.000000000000000000, -0.2064631973583561375 ) ) ;
#12807 = AXIS2_PLACEMENT_3D ( 'NONE', #9488, #21535, #2867 ) ;
#12808 = EDGE_LOOP ( 'NONE', ( #12970, #4466, #2176, #11463 ) ) ;
#12809 = CYLINDRICAL_SURFACE ( 'NONE', #20946, 0.7950199999999985057 ) ;
#12810 = CARTESIAN_POINT ( 'NONE',  ( 37.19264538843808765, -6.356984999999999886, -4.718486965773546871 ) ) ;
#12811 = EDGE_LOOP ( 'NONE', ( #12769, #18787, #9256, #443 ) ) ;
#12812 = ORIENTED_EDGE ( 'NONE', *, *, #16138, .F. ) ;
#12813 = VECTOR ( 'NONE', #18594, 1000.000000000000114 ) ;
#12814 = CARTESIAN_POINT ( 'NONE',  ( 30.10940225190841701, 29.71825598581263961, -2.349505688218141319 ) ) ;
#12816 = CARTESIAN_POINT ( 'NONE',  ( 28.87608719841374949, 29.75832250000000201, -15.73691681567849976 ) ) ;
#12815 = CARTESIAN_POINT ( 'NONE',  ( 6.867032585371679154, 20.09449018309318191, 7.026303756821641322 ) ) ;
#12817 = EDGE_LOOP ( 'NONE', ( #16435, #3442, #6517, #5387 ) ) ;
#12818 = CARTESIAN_POINT ( 'NONE',  ( 3.961642205674128281, 19.15682536790682633, -0.6604031723089509587 ) ) ;
#12819 = EDGE_CURVE ( 'NONE', #11144, #21347, #965, .T. ) ;
#12820 = ORIENTED_EDGE ( 'NONE', *, *, #16460, .T. ) ;
#12821 = EDGE_CURVE ( 'NONE', #16035, #13814, #17488, .T. ) ;
#12822 = VERTEX_POINT ( 'NONE', #10844 ) ;
#12823 = CARTESIAN_POINT ( 'NONE',  ( 0.7634208374692786903, 12.21449189027183202, 4.858061345911853124 ) ) ;
#12824 = VECTOR ( 'NONE', #15910, 1000.000000000000114 ) ;
#12825 = VERTEX_POINT ( 'NONE', #17592 ) ;
#12826 = CARTESIAN_POINT ( 'NONE',  ( 2.861593723304581616, 12.14881861375367755, 5.191963922796355213 ) ) ;
#12827 = VECTOR ( 'NONE', #13110, 1000.000000000000000 ) ;
#12828 = AXIS2_PLACEMENT_3D ( 'NONE', #14661, #21367, #4686 ) ;
#12829 = CYLINDRICAL_SURFACE ( 'NONE', #17738, 1.983739999999995618 ) ;
#12830 = CARTESIAN_POINT ( 'NONE',  ( 39.72849559140086484, 38.13028898904873643, -3.181773261539532438 ) ) ;
#12831 = CARTESIAN_POINT ( 'NONE',  ( 65.64431122251959039, 1.984375000000000000, -11.29787305743958115 ) ) ;
#12832 = DIRECTION ( 'NONE',  ( 0.9579671649362033747, 0.000000000000000000, -0.2868778675745011220 ) ) ;
#12833 = CARTESIAN_POINT ( 'NONE',  ( 3.650877847608121840, 15.06301662852333578, 9.047293290129529097 ) ) ;
#12834 = ORIENTED_EDGE ( 'NONE', *, *, #5765, .F. ) ;
#12835 = DIRECTION ( 'NONE',  ( 0.000000000000000000, -1.000000000000000000, 0.000000000000000000 ) ) ;
#12836 = DIRECTION ( 'NONE',  ( 0.000000000000000000, 1.000000000000000000, 0.000000000000000000 ) ) ;
#12837 = CARTESIAN_POINT ( 'NONE',  ( 13.32162806899934893, 21.37707596500918683, 1.856000767176475552 ) ) ;
#12838 = CARTESIAN_POINT ( 'NONE',  ( 46.03750000000000142, 36.51313500000000545, -10.31874999999999964 ) ) ;
#12839 = VECTOR ( 'NONE', #12835, 1000.000000000000000 ) ;
#12840 = ORIENTED_EDGE ( 'NONE', *, *, #2080, .F. ) ;
#12841 = ORIENTED_EDGE ( 'NONE', *, *, #2922, .F. ) ;
#12842 = CARTESIAN_POINT ( 'NONE',  ( 12.03032088244432707, 10.82393886236346248, 2.770426701479023812 ) ) ;
#12844 = CARTESIAN_POINT ( 'NONE',  ( 1.670997140563193373, -1.594802499999999013, -22.76294857149378714 ) ) ;
#12843 = CARTESIAN_POINT ( 'NONE',  ( 21.25660046192028929, 36.51313500000000545, -13.18703856829094079 ) ) ;
#12845 = CARTESIAN_POINT ( 'NONE',  ( 11.53638331813690954, 20.03120816360499745, -3.140810468174559222 ) ) ;
#12846 = ORIENTED_EDGE ( 'NONE', *, *, #15634, .F. ) ;
#12847 = ORIENTED_EDGE ( 'NONE', *, *, #4771, .T. ) ;
#12848 = EDGE_CURVE ( 'NONE', #11872, #18115, #12620, .T. ) ;
#12849 = DIRECTION ( 'NONE',  ( -0.8558687090795834562, 0.000000000000000000, 0.5171931484643310650 ) ) ;
#12850 = CARTESIAN_POINT ( 'NONE',  ( 7.216176021458938550, 15.38174918897333221, -2.804623791465954863 ) ) ;
#12851 = AXIS2_PLACEMENT_3D ( 'NONE', #20440, #18366, #10297 ) ;
#12852 = CIRCLE ( 'NONE', #2944, 1.587499999999998579 ) ;
#12853 = DIRECTION ( 'NONE',  ( 0.000000000000000000, -1.000000000000000000, -0.000000000000000000 ) ) ;
#12854 = CARTESIAN_POINT ( 'NONE',  ( 8.038529297171338683, 20.58475548577969150, 4.525697635533767027 ) ) ;
#12855 = CARTESIAN_POINT ( 'NONE',  ( 2.817889642889978674, 19.15467982449370510, 7.378628536716077768 ) ) ;
#12856 = VECTOR ( 'NONE', #20628, 1000.000000000000114 ) ;
#12857 = CARTESIAN_POINT ( 'NONE',  ( 10.40160824207624124, 10.44972119249194087, 2.176742725712211612 ) ) ;
#12858 = DIRECTION ( 'NONE',  ( 0.000000000000000000, -1.000000000000000000, 0.000000000000000000 ) ) ;
#12859 = CARTESIAN_POINT ( 'NONE',  ( 49.13030338002142372, 109.3223030719999969, -2.154981381712871791 ) ) ;
#12860 = CARTESIAN_POINT ( 'NONE',  ( 4.982336563036975363, 11.34978398626420137, 5.629178714701890129 ) ) ;
#12861 = CARTESIAN_POINT ( 'NONE',  ( 1.696998172421366080, 15.65649341095878455, 9.566233938423973626 ) ) ;
#12862 = AXIS2_PLACEMENT_3D ( 'NONE', #15461, #6819, #6710 ) ;
#12863 = CARTESIAN_POINT ( 'NONE',  ( 11.81489480602983733, -4.423560566030109165, -15.68132100204162249 ) ) ;
#12864 = CARTESIAN_POINT ( 'NONE',  ( 1.586865396680246620, 15.70174598044015291, 8.856975764382001515 ) ) ;
#12865 = CARTESIAN_POINT ( 'NONE',  ( 29.64606458365116737, -6.752907499999998286, -15.53894806404596096 ) ) ;
#12866 = DIRECTION ( 'NONE',  ( 0.8667647648559581031, 0.000000000000000000, 0.4987171968201974948 ) ) ;
#12867 = CARTESIAN_POINT ( 'NONE',  ( 17.85888992747382886, -7.950010299323909457, -14.45371996643464918 ) ) ;
#12868 = EDGE_LOOP ( 'NONE', ( #9368, #12377, #2305, #21724 ) ) ;
#12869 = CARTESIAN_POINT ( 'NONE',  ( 34.84490081146155660, 34.52875999999999834, -0.2108409695808725060 ) ) ;
#12870 = CARTESIAN_POINT ( 'NONE',  ( 9.155526609938167582, 17.09045796635639647, -3.577556058969439956 ) ) ;
#12871 = ORIENTED_EDGE ( 'NONE', *, *, #14923, .F. ) ;
#12872 = AXIS2_PLACEMENT_3D ( 'NONE', #20994, #18888, #13952 ) ;
#12873 = DIRECTION ( 'NONE',  ( -0.9685006480810791629, 4.068963411654120556E-16, -0.2490110332224850231 ) ) ;
#12874 = EDGE_CURVE ( 'NONE', #4408, #21155, #19343, .T. ) ;
#12875 = CARTESIAN_POINT ( 'NONE',  ( 5.708262345184669684, 12.06421266500533385, -0.1129897529190057592 ) ) ;
#12876 = DIRECTION ( 'NONE',  ( 0.08420877549337300871, 0.000000000000000000, 0.9964481331860212121 ) ) ;
#12877 = CARTESIAN_POINT ( 'NONE',  ( 4.018752164006647476, 18.69182423982057273, -0.1184710799488992716 ) ) ;
#12878 = EDGE_LOOP ( 'NONE', ( #1598, #16588, #7502, #542 ) ) ;
#12879 = CARTESIAN_POINT ( 'NONE',  ( 65.47912282493159353, 0.000000000000000000, -13.30734117861468135 ) ) ;
#12880 = FACE_OUTER_BOUND ( 'NONE', #4972, .T. ) ;
#12881 = AXIS2_PLACEMENT_3D ( 'NONE', #19552, #4419, #16144 ) ;
#12882 = CARTESIAN_POINT ( 'NONE',  ( 9.503420364428157185, 13.29753225131360139, 6.313021545593930028 ) ) ;
#12883 = AXIS2_PLACEMENT_3D ( 'NONE', #17526, #1030, #704 ) ;
#12884 = LINE ( 'NONE', #11203, #11071 ) ;
#12885 = CARTESIAN_POINT ( 'NONE',  ( 71.03963378001139972, 30.56064500000000095, -10.54138470677948014 ) ) ;
#12886 = CARTESIAN_POINT ( 'NONE',  ( -13.49374999999999858, 0.000000000000000000, 0.000000000000000000 ) ) ;
#12887 = CARTESIAN_POINT ( 'NONE',  ( 57.69402548289047417, 34.52875999999999834, -20.84562559047711261 ) ) ;
#12888 = DIRECTION ( 'NONE',  ( 0.07875956036501312318, 0.000000000000000000, -0.9968936410927243807 ) ) ;
#12889 = ADVANCED_FACE ( 'NONE', ( #5963 ), #188, .F. ) ;
#12890 = CARTESIAN_POINT ( 'NONE',  ( 20.64792629172051974, -5.531186785911284431, -15.09723995909050309 ) ) ;
#12891 = DIRECTION ( 'NONE',  ( 0.9237641507921645623, 0.000000000000000000, 0.3829618697876213673 ) ) ;
#12892 = VERTEX_POINT ( 'NONE', #295 ) ;
#12893 = DIRECTION ( 'NONE',  ( 0.000000000000000000, -1.000000000000000000, -0.000000000000000000 ) ) ;
#12894 = VECTOR ( 'NONE', #10081, 1000.000000000000114 ) ;
#12895 = CARTESIAN_POINT ( 'NONE',  ( 38.82016491058538321, 42.06303499999999929, -14.75770094105646812 ) ) ;
#12896 = ORIENTED_EDGE ( 'NONE', *, *, #14517, .F. ) ;
#12897 = EDGE_CURVE ( 'NONE', #21869, #4861, #20713, .T. ) ;
#12898 = CARTESIAN_POINT ( 'NONE',  ( 10.44085112785771940, 20.71911837938399970, -0.3471262034279907205 ) ) ;
#12899 = CARTESIAN_POINT ( 'NONE',  ( 53.08681243026497043, 37.69777154208443193, -16.72443647847455850 ) ) ;
#12900 = CARTESIAN_POINT ( 'NONE',  ( 1.037299993275809129, 18.58659267166814999, 8.184560022580539496 ) ) ;
#12901 = EDGE_CURVE ( 'NONE', #3881, #13013, #17202, .T. ) ;
#12902 = ADVANCED_FACE ( 'NONE', ( #8588, #13589, #20291 ), #10470, .F. ) ;
#12903 = CARTESIAN_POINT ( 'NONE',  ( 17.51061561465282068, -8.559080621069766082, -15.60190410038134878 ) ) ;
#12904 = CARTESIAN_POINT ( 'NONE',  ( 43.49132289107146931, 34.52875999999999834, 4.686923926377883021 ) ) ;
#12905 = ORIENTED_EDGE ( 'NONE', *, *, #15321, .T. ) ;
#12906 =( NAMED_UNIT ( * ) PLANE_ANGLE_UNIT ( ) SI_UNIT ( $, .RADIAN. ) );
#12907 = CIRCLE ( 'NONE', #5825, 1.785937499999998179 ) ;
#12908 = CARTESIAN_POINT ( 'NONE',  ( 43.47225467835515644, -6.356984999999999886, -9.606390615345221207 ) ) ;
#12909 = DIRECTION ( 'NONE',  ( 0.6050250551579474667, 0.7753173868113220069, -0.1811839737371539749 ) ) ;
#12910 = EDGE_LOOP ( 'NONE', ( #4282, #12924, #7052, #5268 ) ) ;
#12911 = CARTESIAN_POINT ( 'NONE',  ( -22.30848347979677371, -1.983740000000001613, 1.064728033956552800 ) ) ;
#12912 = CARTESIAN_POINT ( 'NONE',  ( 0.4797181036071520022, 18.70046581331961377, 1.488109832587226400 ) ) ;
#12913 = ORIENTED_EDGE ( 'NONE', *, *, #15186, .F. ) ;
#12914 = CARTESIAN_POINT ( 'NONE',  ( 13.04981212868784546, 13.21942167511952171, 5.527924531863672719 ) ) ;
#12915 = CARTESIAN_POINT ( 'NONE',  ( 61.83151161312219557, -1.983739999999999837, -0.3645647634491749334 ) ) ;
#12916 = CARTESIAN_POINT ( 'NONE',  ( 10.76563475082845045, 10.89862672135422095, 4.180636303131555209 ) ) ;
#12917 = EDGE_CURVE ( 'NONE', #2958, #8281, #8796, .T. ) ;
#12918 = CARTESIAN_POINT ( 'NONE',  ( 20.03282866373563209, -3.767791603764007125, -15.31592657159819204 ) ) ;
#12919 = DIRECTION ( 'NONE',  ( 0.000000000000000000, 1.000000000000000000, 0.000000000000000000 ) ) ;
#12920 = ORIENTED_EDGE ( 'NONE', *, *, #19165, .F. ) ;
#12921 = CARTESIAN_POINT ( 'NONE',  ( 6.937125200865347452, 11.28756208157694019, 5.042906767430812565 ) ) ;
#12922 = CARTESIAN_POINT ( 'NONE',  ( 55.52866846859685523, -14.84248999999999974, -11.12083858657437752 ) ) ;
#12923 = ORIENTED_EDGE ( 'NONE', *, *, #15321, .F. ) ;
#12924 = ORIENTED_EDGE ( 'NONE', *, *, #17206, .T. ) ;
#12925 = CYLINDRICAL_SURFACE ( 'NONE', #12746, 0.5080000000000013394 ) ;
#12926 = EDGE_CURVE ( 'NONE', #11999, #9809, #6957, .T. ) ;
#12928 = LINE ( 'NONE', #10920, #4966 ) ;
#12927 = CARTESIAN_POINT ( 'NONE',  ( 3.693057765962900696, 14.72322116853433194, 9.052632804461167026 ) ) ;
#12929 = ORIENTED_EDGE ( 'NONE', *, *, #13815, .T. ) ;
#12930 = CARTESIAN_POINT ( 'NONE',  ( 3.966093002749460972, 11.78989785928834166, 1.136079879895026457 ) ) ;
#12931 = ORIENTED_EDGE ( 'NONE', *, *, #6729, .T. ) ;
#12932 = ORIENTED_EDGE ( 'NONE', *, *, #1883, .T. ) ;
#12933 = AXIS2_PLACEMENT_3D ( 'NONE', #19029, #16936, #18700 ) ;
#12934 = CARTESIAN_POINT ( 'NONE',  ( 1.031545730800382143, 12.42199107967254612, 6.104814753628482471 ) ) ;
#12935 = ORIENTED_EDGE ( 'NONE', *, *, #12412, .F. ) ;
#12936 = CARTESIAN_POINT ( 'NONE',  ( 4.271378093513435559, 12.07963554767070491, 2.399734011776157860 ) ) ;
#12937 = CARTESIAN_POINT ( 'NONE',  ( 52.19198938901277529, 34.52875999999999834, 3.449560060533523487 ) ) ;
#12938 = EDGE_CURVE ( 'NONE', #6597, #15472, #10698, .T. ) ;
#12939 = LINE ( 'NONE', #14604, #17076 ) ;
#12940 = CARTESIAN_POINT ( 'NONE',  ( 49.28028498622276032, 0.000000000000000000, -25.68670502218146368 ) ) ;
#12941 = CARTESIAN_POINT ( 'NONE',  ( 36.73521423675246922, 0.000000000000000000, 2.413462327205186497 ) ) ;
#12942 = CARTESIAN_POINT ( 'NONE',  ( 2.952410920574639164, 11.41616042669180153, 5.536812326145255980 ) ) ;
#12943 = ADVANCED_FACE ( 'NONE', ( #11911 ), #15366, .F. ) ;
#12944 = EDGE_CURVE ( 'NONE', #13358, #20009, #3624, .T. ) ;
#12945 = EDGE_LOOP ( 'NONE', ( #13422, #14803, #2728, #4557 ) ) ;
#12946 = CARTESIAN_POINT ( 'NONE',  ( 49.13030338002142372, 34.52875999999999834, -2.154981381712871791 ) ) ;
#12947 = DIRECTION ( 'NONE',  ( 0.8943161143440100380, 0.000000000000000000, 0.4474356798743612806 ) ) ;
#12948 = DIRECTION ( 'NONE',  ( 0.000000000000000000, 0.000000000000000000, -1.000000000000000000 ) ) ;
#12949 = SURFACE_STYLE_USAGE ( .BOTH. , #4313 ) ;
#12950 = DIRECTION ( 'NONE',  ( 0.000000000000000000, 1.000000000000000000, 0.000000000000000000 ) ) ;
#12951 = VERTEX_POINT ( 'NONE', #10366 ) ;
#12952 = VERTEX_POINT ( 'NONE', #18868 ) ;
#12953 = CARTESIAN_POINT ( 'NONE',  ( 11.13175442624480027, 11.34274383772578254, -1.019214542774232291 ) ) ;
#12955 = CYLINDRICAL_SURFACE ( 'NONE', #12797, 0.7950200000000005041 ) ;
#12954 = LINE ( 'NONE', #19662, #8348 ) ;
#12956 = CARTESIAN_POINT ( 'NONE',  ( 12.15966635475609436, 21.49276353786485316, -1.487043894966438629 ) ) ;
#12957 = VERTEX_POINT ( 'NONE', #18753 ) ;
#12958 = ORIENTED_EDGE ( 'NONE', *, *, #11727, .T. ) ;
#12959 = DIRECTION ( 'NONE',  ( 0.9790635044817341814, 0.000000000000000000, -0.2035550397114870014 ) ) ;
#12960 = CARTESIAN_POINT ( 'NONE',  ( 8.530860809380452991, 21.37506940292296065, 0.1456188494152097501 ) ) ;
#12961 = CARTESIAN_POINT ( 'NONE',  ( 6.953635458187449103, 20.71811460043715414, 1.644380932150268482 ) ) ;
#12962 = CARTESIAN_POINT ( 'NONE',  ( 2.950444939269316613, 18.77528755091357482, 7.687626738347391075 ) ) ;
#12963 = LINE ( 'NONE', #2774, #11799 ) ;
#12964 = DIRECTION ( 'NONE',  ( 0.2490110332224850231, 0.000000000000000000, -0.9685006480810791629 ) ) ;
#12965 = FACE_BOUND ( 'NONE', #10405, .T. ) ;
#12966 = CARTESIAN_POINT ( 'NONE',  ( 0.4897477519866756390, 11.56708685249278190, 3.664773833674189518 ) ) ;
#12967 = EDGE_CURVE ( 'NONE', #10050, #7705, #9712, .T. ) ;
#12968 = CARTESIAN_POINT ( 'NONE',  ( -17.46249999999999858, 32.54247999999999763, 0.000000000000000000 ) ) ;
#12969 = AXIS2_PLACEMENT_3D ( 'NONE', #21871, #18236, #14944 ) ;
#12970 = ORIENTED_EDGE ( 'NONE', *, *, #3304, .T. ) ;
#12971 = CARTESIAN_POINT ( 'NONE',  ( 3.277779626878584818, 17.95937840445101230, 8.190852587568969057 ) ) ;
#12972 = LINE ( 'NONE', #4340, #1764 ) ;
#12973 = DIRECTION ( 'NONE',  ( 0.7421532822901579785, 0.000000000000000000, -0.6702301885068630005 ) ) ;
#12974 = CARTESIAN_POINT ( 'NONE',  ( 11.08661322212816458, -5.636319538762833758, -15.90164728704758801 ) ) ;
#12975 = ORIENTED_EDGE ( 'NONE', *, *, #18264, .F. ) ;
#12976 = DIRECTION ( 'NONE',  ( -0.9987059298363656357, 0.000000000000000000, -0.05085730733808393328 ) ) ;
#12977 = CARTESIAN_POINT ( 'NONE',  ( 8.123211010957181344, 21.33440546750962241, 5.089800795509036746 ) ) ;
#12978 = CARTESIAN_POINT ( 'NONE',  ( 10.47045210838663465, 21.61076908352683290, -0.3286064108336465561 ) ) ;
#12979 = EDGE_LOOP ( 'NONE', ( #7553, #16899, #273, #11468 ) ) ;
#12980 = CARTESIAN_POINT ( 'NONE',  ( 31.75000000000000000, 0.000000000000000000, -4.317999999999999616 ) ) ;
#12981 = CARTESIAN_POINT ( 'NONE',  ( 11.45073599112340190, 18.47806154431882675, -3.160592916386676610 ) ) ;
#12982 = CARTESIAN_POINT ( 'NONE',  ( 7.324935168321892398, 21.70618499363874321, 2.622908559674388407 ) ) ;
#12983 = CARTESIAN_POINT ( 'NONE',  ( 30.10940225190841701, 29.71825598581263961, -2.349505688218141319 ) ) ;
#12984 = CARTESIAN_POINT ( 'NONE',  ( 4.869080998300100660, 18.75692939610809162, 7.455446531200784044 ) ) ;
#12985 = LINE ( 'NONE', #16301, #16946 ) ;
#12986 = CARTESIAN_POINT ( 'NONE',  ( 6.424002077374439068, 19.97927104947973476, 5.816179246968293803 ) ) ;
#12987 = CIRCLE ( 'NONE', #13347, 1.587500000000000355 ) ;
#12988 = B_SPLINE_CURVE_WITH_KNOTS ( 'NONE', 3,
 ( #2594, #18969, #7889, #12777, #4473, #11208 ),
 .UNSPECIFIED., .F., .F.,
 ( 4, 1, 1, 4 ),
 ( 0.000000000000000000, 0.2500007535536921122, 0.5000000202745886746, 0.5007142149769521211 ),
 .UNSPECIFIED. ) ;
#12989 = CARTESIAN_POINT ( 'NONE',  ( 23.95208767691813279, 23.80367230640320031, -0.5056039973118116038 ) ) ;
#12990 = VERTEX_POINT ( 'NONE', #409 ) ;
#12991 = CARTESIAN_POINT ( 'NONE',  ( 46.03750000000000142, 0.000000000000000000, -10.31874999999999964 ) ) ;
#12992 = CARTESIAN_POINT ( 'NONE',  ( 8.941503686131628825, 19.69124030533750158, 6.014763436590002676 ) ) ;
#12993 = CARTESIAN_POINT ( 'NONE',  ( 4.701704227727827146, 20.47280481670116359, 0.3545505907435208548 ) ) ;
#12994 = PLANE ( 'NONE',  #462 ) ;
#12995 = EDGE_CURVE ( 'NONE', #15022, #10134, #19319, .T. ) ;
#12996 = CARTESIAN_POINT ( 'NONE',  ( 32.52436584422698473, 32.54502000000000095, 1.884807767196291284 ) ) ;
#12997 = CARTESIAN_POINT ( 'NONE',  ( 6.766171957887571864, 11.28156526743874188, 2.705201495196027039 ) ) ;
#12998 = CARTESIAN_POINT ( 'NONE',  ( 2.063750000000000195, 2.380615000000000148, 8.335010000000000474 ) ) ;
#12999 = CARTESIAN_POINT ( 'NONE',  ( 21.15028308705900884, -4.113433257334989435, -15.02320902816535053 ) ) ;
#13000 = DIRECTION ( 'NONE',  ( 0.000000000000000000, 1.000000000000000000, 0.000000000000000000 ) ) ;
#13001 = AXIS2_PLACEMENT_3D ( 'NONE', #2730, #14039, #20744 ) ;
#13002 = ORIENTED_EDGE ( 'NONE', *, *, #14127, .T. ) ;
#13003 = CYLINDRICAL_SURFACE ( 'NONE', #11041, 0.5080000000000005622 ) ;
#13004 = DIRECTION ( 'NONE',  ( 0.000000000000000000, -1.000000000000000000, 0.000000000000000000 ) ) ;
#13005 = EDGE_CURVE ( 'NONE', #11503, #7489, #19661, .T. ) ;
#13006 = ADVANCED_BREP_SHAPE_REPRESENTATION ( '', ( #5939, #2234 ), #3303 ) ;
#13007 = ORIENTED_EDGE ( 'NONE', *, *, #19891, .F. ) ;
#13008 = CARTESIAN_POINT ( 'NONE',  ( 10.76378183054590920, 21.07819761844824313, 0.5131835306795289320 ) ) ;
#13009 = CARTESIAN_POINT ( 'NONE',  ( 28.97711086133420366, 0.000000000000000000, -10.31874999999999964 ) ) ;
#13010 = CARTESIAN_POINT ( 'NONE',  ( -0.1152391821539391209, 20.23795519954344613, 5.330493952060566976 ) ) ;
#13011 = CARTESIAN_POINT ( 'NONE',  ( 17.94914520215607823, -8.292551780608357959, -14.46302984805736003 ) ) ;
#13012 = DIRECTION ( 'NONE',  ( -0.7421532822901580895, 0.000000000000000000, 0.6702301885068630005 ) ) ;
#13013 = VERTEX_POINT ( 'NONE', #5259 ) ;
#13014 = DIRECTION ( 'NONE',  ( 0.6287118719681975554, 0.000000000000000000, 0.7776383362760898033 ) ) ;
#13015 = ORIENTED_EDGE ( 'NONE', *, *, #10215, .F. ) ;
#13016 = CARTESIAN_POINT ( 'NONE',  ( 22.05855709630448303, 26.98019749999999917, -44.85793026951184004 ) ) ;
#13017 = AXIS2_PLACEMENT_3D ( 'NONE', #15179, #11851, #4882 ) ;
#13018 = ORIENTED_EDGE ( 'NONE', *, *, #13043, .T. ) ;
#13019 = CARTESIAN_POINT ( 'NONE',  ( 11.11705324017706786, 16.27078922038442599, -3.687858511736137768 ) ) ;
#13020 = CARTESIAN_POINT ( 'NONE',  ( 19.99312429566830218, -3.968114999999999615, -11.46559883803463720 ) ) ;
#13021 = CARTESIAN_POINT ( 'NONE',  ( 10.59745498212427073, 21.89042938493124169, 0.06821599229823353816 ) ) ;
#13022 = EDGE_CURVE ( 'NONE', #1096, #20415, #17327, .T. ) ;
#13023 = EDGE_CURVE ( 'NONE', #8453, #20325, #21085, .T. ) ;
#13024 = APPLICATION_CONTEXT ( 'automotive_design' ) ;
#13025 = CARTESIAN_POINT ( 'NONE',  ( 19.98943338725409546, -4.012182358950986405, -15.31543382922598262 ) ) ;
#13026 = DIRECTION ( 'NONE',  ( 0.000000000000000000, 1.000000000000000000, 0.000000000000000000 ) ) ;
#13027 = VERTEX_POINT ( 'NONE', #5380 ) ;
#13028 = DIRECTION ( 'NONE',  ( -0.9685006480810794960, 0.000000000000000000, -0.2490110332224836354 ) ) ;
#13029 = CARTESIAN_POINT ( 'NONE',  ( -1.848761088705630051, 9.129395000000000593, 7.884515871828260636 ) ) ;
#13030 = ORIENTED_EDGE ( 'NONE', *, *, #18597, .F. ) ;
#13031 = EDGE_LOOP ( 'NONE', ( #12281, #18196, #17555, #18619 ) ) ;
#13032 = AXIS2_PLACEMENT_3D ( 'NONE', #9119, #14132, #15900 ) ;
#13033 = FACE_OUTER_BOUND ( 'NONE', #5288, .T. ) ;
#13034 = CARTESIAN_POINT ( 'NONE',  ( 5.550556903167823464, 21.64685404058683815, 3.813055932019618677 ) ) ;
#13035 = ORIENTED_EDGE ( 'NONE', *, *, #9921, .T. ) ;
#13036 = CARTESIAN_POINT ( 'NONE',  ( 3.815750765661552357, 12.28651131542703112, 0.4528471948513508871 ) ) ;
#13037 = EDGE_LOOP ( 'NONE', ( #16885, #16843, #4475, #14177 ) ) ;
#13038 = VERTEX_POINT ( 'NONE', #6829 ) ;
#13039 = ADVANCED_FACE ( 'NONE', ( #15250 ), #77, .F. ) ;
#13040 = EDGE_CURVE ( 'NONE', #17367, #13795, #20846, .T. ) ;
#13041 = VERTEX_POINT ( 'NONE', #853 ) ;
#13042 = AXIS2_PLACEMENT_3D ( 'NONE', #11382, #16690, #8372 ) ;
#13043 = EDGE_CURVE ( 'NONE', #11383, #4031, #19408, .T. ) ;
#13044 = CARTESIAN_POINT ( 'NONE',  ( 38.23013820809905638, 32.54502000000000095, -14.22485453658974031 ) ) ;
#13045 = DIRECTION ( 'NONE',  ( 0.000000000000000000, 1.000000000000000000, 0.000000000000000000 ) ) ;
#13046 = DIRECTION ( 'NONE',  ( 0.000000000000000000, 0.000000000000000000, 1.000000000000000000 ) ) ;
#13047 = PRODUCT_DEFINITION_SHAPE ( 'NONE', 'NONE',  #18695 ) ;
#13048 = FACE_OUTER_BOUND ( 'NONE', #4630, .T. ) ;
#13049 = CARTESIAN_POINT ( 'NONE',  ( 2.278003711904815987, 11.54516833574618317, 2.618891172102409293 ) ) ;
#13050 = ORIENTED_EDGE ( 'NONE', *, *, #20215, .T. ) ;
#13051 = CARTESIAN_POINT ( 'NONE',  ( 42.79471501377724252, 34.52875999999999834, 5.049205022181460834 ) ) ;
#13052 = CYLINDRICAL_SURFACE ( 'NONE', #6771, 0.5079999999999996740 ) ;
#13053 = CARTESIAN_POINT ( 'NONE',  ( 29.36874999999999858, 0.000000000000000000, -10.31874999999999964 ) ) ;
#13054 = DIRECTION ( 'NONE',  ( 0.000000000000000000, 1.000000000000000000, 0.000000000000000000 ) ) ;
#13055 = VECTOR ( 'NONE', #2247, 1000.000000000000227 ) ;
#13056 = CARTESIAN_POINT ( 'NONE',  ( -15.39353573898878658, -4.587157632697119958, -10.30107656633069979 ) ) ;
#13057 = EDGE_CURVE ( 'NONE', #20317, #16343, #17909, .T. ) ;
#13058 = ORIENTED_EDGE ( 'NONE', *, *, #2345, .F. ) ;
#13059 = ORIENTED_EDGE ( 'NONE', *, *, #11028, .F. ) ;
#13060 = CARTESIAN_POINT ( 'NONE',  ( 7.125560052436228808, 16.36585256730476701, -2.220941111682218416 ) ) ;
#13061 = DIRECTION ( 'NONE',  ( 0.000000000000000000, -1.000000000000000000, 0.000000000000000000 ) ) ;
#13062 = ORIENTED_EDGE ( 'NONE', *, *, #18968, .F. ) ;
#13063 = ORIENTED_EDGE ( 'NONE', *, *, #6830, .F. ) ;
#13064 = DIRECTION ( 'NONE',  ( 1.000000000000000000, 0.000000000000000000, 0.000000000000000000 ) ) ;
#13065 = AXIS2_PLACEMENT_3D ( 'NONE', #19087, #12480, #4068 ) ;
#13066 = EDGE_CURVE ( 'NONE', #2577, #4289, #12987, .T. ) ;
#13067 = CARTESIAN_POINT ( 'NONE',  ( 8.695075460036933990, 19.30551093097031412, 6.194751677661820111 ) ) ;
#13068 = EDGE_CURVE ( 'NONE', #3226, #6728, #12264, .T. ) ;
#13069 = CIRCLE ( 'NONE', #2463, 1.785937499999998179 ) ;
#13070 = EDGE_CURVE ( 'NONE', #15859, #93, #4146, .T. ) ;
#13071 = CARTESIAN_POINT ( 'NONE',  ( 3.376984682214053013, 16.43012674869273582, 8.444289425429094109 ) ) ;
#13072 = VECTOR ( 'NONE', #18167, 1000.000000000000000 ) ;
#13073 = CARTESIAN_POINT ( 'NONE',  ( 30.25543876212147509, 32.54502000000000095, -19.39939755251907272 ) ) ;
#13074 = CARTESIAN_POINT ( 'NONE',  ( 27.87822510359947614, 2.586003464000000029, -8.893823290944665061 ) ) ;
#13075 = DIRECTION ( 'NONE',  ( 0.4128958666089267981, -0.5884034904305870395, -0.6951966166390379787 ) ) ;
#13076 = CARTESIAN_POINT ( 'NONE',  ( 0.6892992815739681367, 11.43080006335364374, 4.536020415443320353 ) ) ;
#13077 = DIRECTION ( 'NONE',  ( 0.1065921516619546816, -0.9937903127262236458, -0.03192064434796833272 ) ) ;
#13078 = ORIENTED_EDGE ( 'NONE', *, *, #11652, .F. ) ;
#13079 = CARTESIAN_POINT ( 'NONE',  ( 1.458656339048537420, 17.15958586172077460, 8.823384646655476615 ) ) ;
#13080 = CARTESIAN_POINT ( 'NONE',  ( 1.537498671273937578, 23.46184445063047974, 10.69425292771247449 ) ) ;
#13081 = CYLINDRICAL_SURFACE ( 'NONE', #8175, 0.7950200000000000600 ) ;
#13082 = CARTESIAN_POINT ( 'NONE',  ( 53.25483508941461963, 34.52875999999999834, -5.879799058943532941 ) ) ;
#13083 = LINE ( 'NONE', #20107, #21843 ) ;
#13084 = VERTEX_POINT ( 'NONE', #11233 ) ;
#13085 = DIRECTION ( 'NONE',  ( -0.6702301885068628895, 0.000000000000000000, -0.7421532822901579785 ) ) ;
#13086 = CARTESIAN_POINT ( 'NONE',  ( 11.92979004589613190, 21.69514399574918073, 3.992311296994946801 ) ) ;
#13087 = VECTOR ( 'NONE', #1947, 1000.000000000000000 ) ;
#13088 = CARTESIAN_POINT ( 'NONE',  ( 9.121940360070944109, 13.82260832479536816, -3.046301295306517165 ) ) ;
#13089 = VERTEX_POINT ( 'NONE', #10807 ) ;
#13090 = CARTESIAN_POINT ( 'NONE',  ( 8.453759634856433891, 20.82441444446472190, 5.697268492166688958 ) ) ;
#13091 = DIRECTION ( 'NONE',  ( 0.2490110332224846346, 0.000000000000000000, -0.9685006480810792739 ) ) ;
#13092 = CARTESIAN_POINT ( 'NONE',  ( 2.854147253460158851, 19.21826933052950181, 7.434877585083132345 ) ) ;
#13093 = ADVANCED_FACE ( 'NONE', ( #4065 ), #21290, .T. ) ;
#13094 = CARTESIAN_POINT ( 'NONE',  ( 1.268730000000000135, 24.21318500000000284, 8.731249999999999289 ) ) ;
#13095 = ADVANCED_FACE ( 'NONE', ( #627 ), #17554, .T. ) ;
#13096 = AXIS2_PLACEMENT_3D ( 'NONE', #8733, #4438, #7633 ) ;
#13097 = CARTESIAN_POINT ( 'NONE',  ( 27.93207353965470574, -1.983739999999999837, -8.388685343514779902 ) ) ;
#13098 = CARTESIAN_POINT ( 'NONE',  ( 9.334231404058437320, 18.26872045576617865, 6.931657937804551750 ) ) ;
#13099 = CIRCLE ( 'NONE', #15208, 4.365624999999999645 ) ;
#13100 = PRESENTATION_LAYER_ASSIGNMENT (  '', '', ( #20112 ) ) ;
#13101 = CARTESIAN_POINT ( 'NONE',  ( 3.873944326939889216, 13.69792732696330262, -0.8314339933664549598 ) ) ;
#13102 = CARTESIAN_POINT ( 'NONE',  ( 0.7843704457339527591, -1.594802499999999013, -23.55949434567611078 ) ) ;
#13103 = FACE_OUTER_BOUND ( 'NONE', #19318, .T. ) ;
#13104 = CARTESIAN_POINT ( 'NONE',  ( 38.94885947252404179, -5.166721542084396823, -3.956611957468594287 ) ) ;
#13105 = DIRECTION ( 'NONE',  ( -0.4987171968201928873, 0.000000000000000000, 0.8667647648559606566 ) ) ;
#13106 = CARTESIAN_POINT ( 'NONE',  ( 12.61411201210553124, 21.25996874134203907, -20.12292187596927562 ) ) ;
#13107 = FACE_BOUND ( 'NONE', #18500, .T. ) ;
#13108 = VECTOR ( 'NONE', #17646, 1000.000000000000000 ) ;
#13109 = VERTEX_POINT ( 'NONE', #15911 ) ;
#13110 = DIRECTION ( 'NONE',  ( -0.08420877549337300871, 0.000000000000000000, -0.9964481331860212121 ) ) ;
#13111 = AXIS2_PLACEMENT_3D ( 'NONE', #5047, #1186, #4731 ) ;
#13112 = CARTESIAN_POINT ( 'NONE',  ( 67.40134256979101224, 0.000000000000000000, -13.30734117861468135 ) ) ;
#13113 = EDGE_LOOP ( 'NONE', ( #15293, #6166, #8683, #17692 ) ) ;
#13114 = CARTESIAN_POINT ( 'NONE',  ( 11.78825387765158972, 20.99241592478037077, 3.275920435853647561 ) ) ;
#13115 = DIRECTION ( 'NONE',  ( 0.2490110332224846623, 0.000000000000000000, -0.9685006480810793850 ) ) ;
#13116 = DIRECTION ( 'NONE',  ( -0.9790635044817341814, 0.000000000000000000, 0.2035550397114869736 ) ) ;
#13117 = CARTESIAN_POINT ( 'NONE',  ( 14.57805970825261355, -7.268432535603025713, -16.41340505930001115 ) ) ;
#13118 = DIRECTION ( 'NONE',  ( 0.000000000000000000, -1.000000000000000000, 0.000000000000000000 ) ) ;
#13119 = ORIENTED_EDGE ( 'NONE', *, *, #19264, .F. ) ;
#13120 = FACE_OUTER_BOUND ( 'NONE', #4429, .T. ) ;
#13121 = ADVANCED_FACE ( 'NONE', ( #4168 ), #11130, .T. ) ;
#13122 = ORIENTED_EDGE ( 'NONE', *, *, #12657, .F. ) ;
#13123 = B_SPLINE_CURVE_WITH_KNOTS ( 'NONE', 3,
 ( #9771, #9667, #13352, #20056, #16770 ),
 .UNSPECIFIED., .F., .F.,
 ( 4, 1, 4 ),
 ( 0.007480389903056189338, 0.007494994329912538743, 0.007509598756768888148 ),
 .UNSPECIFIED. ) ;
#13124 = CARTESIAN_POINT ( 'NONE',  ( 52.91086381164393515, 34.52875999999999834, 3.812938856729753301 ) ) ;
#13125 = CARTESIAN_POINT ( 'NONE',  ( 0.8312686293824771422, 19.60397523007529230, 2.320213228409029327 ) ) ;
#13126 = VECTOR ( 'NONE', #3154, 1000.000000000000227 ) ;
#13127 = CIRCLE ( 'NONE', #14542, 0.5953125000000000222 ) ;
#13128 = ORIENTED_EDGE ( 'NONE', *, *, #1948, .T. ) ;
#13129 = CARTESIAN_POINT ( 'NONE',  ( 9.640329918106763429, 18.90712183571880090, -2.306490695281333547 ) ) ;
#13130 = CARTESIAN_POINT ( 'NONE',  ( 2.873684328219870743, 20.03727096405572539, 2.085104636573927195 ) ) ;
#13131 = AXIS2_PLACEMENT_3D ( 'NONE', #20466, #5018, #3471 ) ;
#13132 = CARTESIAN_POINT ( 'NONE',  ( 38.31330449142736683, 39.48727169022187411, -4.745061478489406959 ) ) ;
#13133 = CARTESIAN_POINT ( 'NONE',  ( 11.15539492206983319, 12.02330533696836135, 5.876692431811527229 ) ) ;
#13134 = CARTESIAN_POINT ( 'NONE',  ( 29.31223750860709742, 2.809619014187358932, -5.011466527456265752 ) ) ;
#13135 = ORIENTED_EDGE ( 'NONE', *, *, #478, .F. ) ;
#13136 = DIRECTION ( 'NONE',  ( -1.000000000000000000, 0.000000000000000000, 0.000000000000000000 ) ) ;
#13137 = CYLINDRICAL_SURFACE ( 'NONE', #18395, 0.5080000000000010063 ) ;
#13138 = ORIENTED_EDGE ( 'NONE', *, *, #4898, .F. ) ;
#13139 = VERTEX_POINT ( 'NONE', #7486 ) ;
#13140 = CIRCLE ( 'NONE', #14565, 2.381250000000001421 ) ;
#13141 = CIRCLE ( 'NONE', #14914, 0.5080000000000014504 ) ;
#13142 = DIRECTION ( 'NONE',  ( -0.9685006480810791629, 0.000000000000000000, -0.2490110332224850231 ) ) ;
#13144 = FACE_OUTER_BOUND ( 'NONE', #20411, .T. ) ;
#13143 = CARTESIAN_POINT ( 'NONE',  ( 1.155066700459650875, 21.11849136136308047, 3.338538337880277762 ) ) ;
#13145 = B_SPLINE_CURVE_WITH_KNOTS ( 'NONE', 3,
 ( #14410, #21125, #12748, #17836, #16180 ),
 .UNSPECIFIED., .F., .F.,
 ( 4, 1, 4 ),
 ( 0.003754349818373685799, 0.003769101685648578240, 0.003783853552923471114 ),
 .UNSPECIFIED. ) ;
#13146 = ORIENTED_EDGE ( 'NONE', *, *, #10292, .F. ) ;
#13147 = CARTESIAN_POINT ( 'NONE',  ( 4.060856035186504620, 11.56482107470509213, 1.554964223477295127 ) ) ;
#13148 = ORIENTED_EDGE ( 'NONE', *, *, #10606, .F. ) ;
#13149 = ADVANCED_FACE ( 'NONE', ( #2727, #14255 ), #20973, .T. ) ;
#13150 = CIRCLE ( 'NONE', #1109, 0.7950200000000003930 ) ;
#13151 = ORIENTED_EDGE ( 'NONE', *, *, #6683, .F. ) ;
#13152 = CARTESIAN_POINT ( 'NONE',  ( 59.65121809612895731, 34.52875999999999834, -2.485718937265306572 ) ) ;
#13153 = EDGE_LOOP ( 'NONE', ( #1171, #5815, #2032, #20407 ) ) ;
#13154 = VECTOR ( 'NONE', #9273, 1000.000000000000114 ) ;
#13155 = AXIS2_PLACEMENT_3D ( 'NONE', #5391, #8602, #8486 ) ;
#13156 = CARTESIAN_POINT ( 'NONE',  ( 19.79515554403045741, 34.52875999999999834, -10.69562145279641996 ) ) ;
#13157 = LINE ( 'NONE', #11151, #18164 ) ;
#13158 = DIRECTION ( 'NONE',  ( 0.08420877549337300871, 0.000000000000000000, 0.9964481331860212121 ) ) ;
#13159 = CARTESIAN_POINT ( 'NONE',  ( 1.966330561627286810, 12.33255769116432177, 1.219573196129033477 ) ) ;
#13160 = CIRCLE ( 'NONE', #19136, 30.16250000000000497 ) ;
#13161 = AXIS2_PLACEMENT_3D ( 'NONE', #11641, #20026, #2808 ) ;
#13162 = ORIENTED_EDGE ( 'NONE', *, *, #1413, .F. ) ;
#13163 = LINE ( 'NONE', #4749, #8933 ) ;
#13164 = CARTESIAN_POINT ( 'NONE',  ( 49.72033008250774344, 42.06303499999999929, -2.687827786179598277 ) ) ;
#13165 = PLANE ( 'NONE',  #15640 ) ;
#13166 = EDGE_CURVE ( 'NONE', #10491, #5733, #3093, .T. ) ;
#13167 = CARTESIAN_POINT ( 'NONE',  ( 53.70970536199543233, 38.15648681541303233, -15.96454499544192096 ) ) ;
#13168 = EDGE_LOOP ( 'NONE', ( #4498, #21004, #19886, #14898, #7501, #7704 ) ) ;
#13169 = VERTEX_POINT ( 'NONE', #21071 ) ;
#13170 = CARTESIAN_POINT ( 'NONE',  ( 6.427231207988340245, 11.74208123617664157, 4.389945309724444300 ) ) ;
#13171 =( BOUNDED_CURVE ( )  B_SPLINE_CURVE ( 3, ( #5158, #3506, #15363, #8267 ),
 .UNSPECIFIED., .F., .F. ) 
 B_SPLINE_CURVE_WITH_KNOTS ( ( 4, 4 ),
 ( 4.712388980381386538, 5.283302931178984529 ),
 .UNSPECIFIED. ) 
 CURVE ( )  GEOMETRIC_REPRESENTATION_ITEM ( )  RATIONAL_B_SPLINE_CURVE ( ( 1.000000000000000000, 0.9730220469480294065, 0.9730220469480294065, 1.000000000000000000 ) ) 
 REPRESENTATION_ITEM ( '' )  );
#13172 = DIRECTION ( 'NONE',  ( 0.7421532822901579785, 0.000000000000000000, -0.6702301885068628895 ) ) ;
#13173 = ORIENTED_EDGE ( 'NONE', *, *, #5550, .F. ) ;
#13174 = CIRCLE ( 'NONE', #16696, 0.7950200000000010592 ) ;
#13175 = ORIENTED_EDGE ( 'NONE', *, *, #12821, .T. ) ;
#13176 = CARTESIAN_POINT ( 'NONE',  ( 65.64431122251959039, 0.000000000000000000, -11.29787305743958115 ) ) ;
#13177 = EDGE_CURVE ( 'NONE', #15380, #12517, #12686, .T. ) ;
#13178 = EDGE_CURVE ( 'NONE', #6430, #5334, #9355, .T. ) ;
#13179 = ADVANCED_FACE ( 'NONE', ( #7699, #14461, #21734 ), #16766, .T. ) ;
#13180 = CARTESIAN_POINT ( 'NONE',  ( 8.201956413317519790, 11.59017961620675052, 1.867525178087086291 ) ) ;
#13181 = CARTESIAN_POINT ( 'NONE',  ( 6.585538771758304932, 11.73707508029471214, 3.688088777089395087 ) ) ;
#13182 = AXIS2_PLACEMENT_3D ( 'NONE', #12240, #10694, #4060 ) ;
#13183 = CIRCLE ( 'NONE', #3637, 0.5080000000000010063 ) ;
#13184 = DIRECTION ( 'NONE',  ( 0.000000000000000000, 1.000000000000000000, 0.000000000000000000 ) ) ;
#13185 = CARTESIAN_POINT ( 'NONE',  ( 28.38195592936287781, 40.07707250000000698, -13.81504834214261024 ) ) ;
#13186 = CARTESIAN_POINT ( 'NONE',  ( 1.702168628018286167, 14.88652389531085163, 9.403711407008401579 ) ) ;
#13187 = LINE ( 'NONE', #8071, #19327 ) ;
#13188 = VERTEX_POINT ( 'NONE', #13134 ) ;
#13189 = CARTESIAN_POINT ( 'NONE',  ( 6.170897731235724493, 20.44464562225766358, 5.225896666988528949 ) ) ;
#13190 = CARTESIAN_POINT ( 'NONE',  ( -2.234700160307072192, 26.98019749999999917, -24.80708529208898483 ) ) ;
#13191 = DIRECTION ( 'NONE',  ( 0.000000000000000000, 1.000000000000000000, 0.000000000000000000 ) ) ;
#13192 = CARTESIAN_POINT ( 'NONE',  ( 11.57594508772183417, -6.391478118055172075, -15.80891331407196354 ) ) ;
#13193 = EDGE_CURVE ( 'NONE', #5628, #12469, #3158, .T. ) ;
#13194 = CARTESIAN_POINT ( 'NONE',  ( 17.87574706213523612, 34.52875999999999834, -11.18912023382283571 ) ) ;
#13195 = ORIENTED_EDGE ( 'NONE', *, *, #9250, .T. ) ;
#13196 = PRODUCT_RELATED_PRODUCT_CATEGORY ( 'part', '', ( #19722 ) ) ;
#13197 = CARTESIAN_POINT ( 'NONE',  ( 11.32818978341159877, 13.68104675248728164, 7.112358373980030457 ) ) ;
#13198 = VECTOR ( 'NONE', #6223, 1000.000000000000114 ) ;
#13199 = CARTESIAN_POINT ( 'NONE',  ( 9.731254064506467572, 20.11182769301898077, -2.300494539041386677 ) ) ;
#13200 = ORIENTED_EDGE ( 'NONE', *, *, #16140, .F. ) ;
#13201 = CARTESIAN_POINT ( 'NONE',  ( 8.972590385489363385, 19.47977362735880291, 7.032588333189179863 ) ) ;
#13202 = FACE_OUTER_BOUND ( 'NONE', #20697, .T. ) ;
#13203 = CARTESIAN_POINT ( 'NONE',  ( 4.439494607601830012, 19.89361395305066083, 0.8919725944796629280 ) ) ;
#13204 = EDGE_CURVE ( 'NONE', #13546, #16767, #8347, .T. ) ;
#13205 = CYLINDRICAL_SURFACE ( 'NONE', #20117, 1.983739999999999393 ) ;
#13206 = AXIS2_PLACEMENT_3D ( 'NONE', #16451, #7921, #19732 ) ;
#13207 = CARTESIAN_POINT ( 'NONE',  ( -22.75431282566211522, 40.79338547039380103, -25.41543459098148716 ) ) ;
#13208 = PLANE ( 'NONE',  #9508 ) ;
#13209 = CARTESIAN_POINT ( 'NONE',  ( 7.841140811635576746, 13.09203250846072208, -1.210482602502612970 ) ) ;
#13210 = DIRECTION ( 'NONE',  ( 0.000000000000000000, 0.000000000000000000, -1.000000000000000000 ) ) ;
#13211 = CARTESIAN_POINT ( 'NONE',  ( 5.639633595010457690, 12.41500460647656112, 7.037384739680620171 ) ) ;
#13212 = DIRECTION ( 'NONE',  ( 0.000000000000000000, 1.000000000000000000, 0.000000000000000000 ) ) ;
#13213 = CARTESIAN_POINT ( 'NONE',  ( 30.02465935949302533, 38.48766750000000059, -2.324128137548288731 ) ) ;
#13214 = CARTESIAN_POINT ( 'NONE',  ( 6.631720943421993475, 11.01939120177532239, 2.726317316095465682 ) ) ;
#13215 = DIRECTION ( 'NONE',  ( 0.000000000000000000, -1.000000000000000000, -0.000000000000000000 ) ) ;
#13216 = CARTESIAN_POINT ( 'NONE',  ( 21.25318714072498594, -3.068702901631692459, -15.03512189218206707 ) ) ;
#13217 = EDGE_CURVE ( 'NONE', #12039, #1153, #13793, .T. ) ;
#13218 = VECTOR ( 'NONE', #16903, 1000.000000000000000 ) ;
#13219 = EDGE_CURVE ( 'NONE', #490, #2577, #18208, .T. ) ;
#13220 = PLANE ( 'NONE',  #10968 ) ;
#13221 = ADVANCED_FACE ( 'NONE', ( #9886 ), #19847, .F. ) ;
#13222 = ORIENTED_EDGE ( 'NONE', *, *, #11915, .T. ) ;
#13223 = CARTESIAN_POINT ( 'NONE',  ( -22.90765545213488963, 43.41875999999999891, -9.869178565316103047 ) ) ;
#13224 = CYLINDRICAL_SURFACE ( 'NONE', #13672, 1.190624999999999822 ) ;
#13225 = VERTEX_POINT ( 'NONE', #11669 ) ;
#13226 = CARTESIAN_POINT ( 'NONE',  ( 12.85077078482076551, 12.25509064126621617, 4.452759652903010235 ) ) ;
#13227 = LINE ( 'NONE', #16431, #16593 ) ;
#13228 = CARTESIAN_POINT ( 'NONE',  ( 6.324617228969283467, 10.93918168731720186, 2.559496390996669923 ) ) ;
#13229 = CARTESIAN_POINT ( 'NONE',  ( 19.42330635861384991, 0.1555817663055659994, -13.72932059668182170 ) ) ;
#13231 = CARTESIAN_POINT ( 'NONE',  ( 31.05388211198297554, 0.000000000000000000, -15.23127950648024331 ) ) ;
#13230 = CARTESIAN_POINT ( 'NONE',  ( 1.042931226275107592, 13.09009564387116065, 7.664567888277438179 ) ) ;
#13232 = AXIS2_PLACEMENT_3D ( 'NONE', #11012, #4274, #7366 ) ;
#13233 = ORIENTED_EDGE ( 'NONE', *, *, #5156, .F. ) ;
#13234 = CYLINDRICAL_SURFACE ( 'NONE', #16981, 4.365625000000000533 ) ;
#13235 = CARTESIAN_POINT ( 'NONE',  ( 4.047143398541026116, 18.29642203768929676, -0.2535756372466432818 ) ) ;
#13236 = EDGE_LOOP ( 'NONE', ( #636, #17368 ) ) ;
#13237 = CARTESIAN_POINT ( 'NONE',  ( 20.22083624039512273, -1.348948031050671847, -14.75776464959390211 ) ) ;
#13238 = CIRCLE ( 'NONE', #12883, 0.5080000000000007843 ) ;
#13239 = CARTESIAN_POINT ( 'NONE',  ( 11.22134872449618825, -3.741537362231782460, -16.47805867944655489 ) ) ;
#13240 = EDGE_LOOP ( 'NONE', ( #5019, #7832, #5515, #5555 ) ) ;
#13241 = CARTESIAN_POINT ( 'NONE',  ( 11.90016014395877342, 20.94917700551698303, 3.661585867165440433 ) ) ;
#13242 = DIRECTION ( 'NONE',  ( -0.7421532822901562021, 0.000000000000000000, 0.6702301885068651099 ) ) ;
#13243 = CARTESIAN_POINT ( 'NONE',  ( 6.758398147623775110, 11.05210752777782091, 4.476560998182233853 ) ) ;
#13244 = AXIS2_PLACEMENT_3D ( 'NONE', #698, #8990, #5890 ) ;
#13245 = CARTESIAN_POINT ( 'NONE',  ( 12.54707462758905834, -5.336976515233779139, -16.77073826699180259 ) ) ;
#13246 = ADVANCED_FACE ( 'NONE', ( #8126 ), #6690, .T. ) ;
#13247 = CARTESIAN_POINT ( 'NONE',  ( 46.03750000000000142, 34.52875999999999834, -10.31874999999999964 ) ) ;
#13248 = ORIENTED_EDGE ( 'NONE', *, *, #11783, .T. ) ;
#13249 = CARTESIAN_POINT ( 'NONE',  ( 9.259384945965678071, 21.08603154913874178, 2.151121503098819332 ) ) ;
#13250 = CARTESIAN_POINT ( 'NONE',  ( 6.065245546251053277, 11.11134465255707937, 1.342380378476411007 ) ) ;
#13251 = FACE_OUTER_BOUND ( 'NONE', #17133, .T. ) ;
#13252 = VECTOR ( 'NONE', #20651, 1000.000000000000000 ) ;
#13253 = ORIENTED_EDGE ( 'NONE', *, *, #11522, .F. ) ;
#13254 = ORIENTED_EDGE ( 'NONE', *, *, #3589, .T. ) ;
#13255 = DIRECTION ( 'NONE',  ( 0.2490110332224846623, 0.000000000000000000, -0.9685006480810793850 ) ) ;
#13257 = CARTESIAN_POINT ( 'NONE',  ( 13.67756757867809725, 12.29391749999999739, 2.571257636385987144 ) ) ;
#13256 = CARTESIAN_POINT ( 'NONE',  ( -0.8081381244975988087, 20.81272068207762516, 3.752964682919363693 ) ) ;
#13258 = ORIENTED_EDGE ( 'NONE', *, *, #1657, .F. ) ;
#13259 = CARTESIAN_POINT ( 'NONE',  ( 7.071627640836038786, 19.23017274739645899, 7.562272307646363600 ) ) ;
#13260 = ORIENTED_EDGE ( 'NONE', *, *, #1953, .T. ) ;
#13261 = B_SPLINE_CURVE_WITH_KNOTS ( 'NONE', 3,
 ( #14990, #14769, #19819, #16314, #21705, #14874, #6453, #13216, #4802, #21266, #4578, #13323, #3034, #12999, #19930, #7781, #4692, #14547, #12890, #21372, #6227, #2930, #9656, #21476, #6333, #11436, #18181, #5117, #17166, #15092, #18814, #134, #3458, #16835, #8647, #13873, #2006, #8746, #5435, #5005, #9984, #15527, #6886, #17053, #21805, #5322, #10193, #356, #15311, #3681, #1580, #11761, #1788, #13646, #18490, #8321, #7104, #18376, #13756, #13535, #15194, #3247, #16740, #16937, #6659, #13419, #20346, #20129, #8531, #3363, #10091, #6769, #1677, #8417, #20452, #5214, #19, #20242, #11970, #18701, #11865, #18591, #12089, #3569, #10310, #1899, #15421, #247, #6985, #14312, #17720, #7549, #20917, #21127, #21029, #19149, #2121, #685, #4118, #910, #2350, #12200, #5779, #7651, #2571, #2238, #14412, #4015, #9080, #3792, #17398, #7430, #17274, #5544, #18922, #5875, #476, #5662, #14090, #14203, #19259, #20795, #15645, #12639, #10528, #12535, #7230, #802, #9188, #10967, #583, #10757, #8861, #13988, #10860, #20687, #7327, #17503, #17606, #15855, #12302, #2460, #15968, #19030, #8976, #19363, #4228, #3904, #12421, #10645, #15756, #9735, #16395, #16287, #11290, #21565, #14745, #14851, #1008, #2896, #1121, #4454, #17937, #19902, #18157, #4776, #19471, #7757, #16605, #8190, #9834, #14641, #17838, #12867, #16182, #11507, #1231, #16498, #11408, #6422, #6096, #4342, #7974, #1443, #19586, #11083, #9517, #9630, #7864, #18040, #21451, #21239, #14964, #19789, #18250, #3109, #5979, #12750, #1333, #14523, #2684, #2782, #11185, #9414, #13192, #21345, #6203, #12974, #6308, #4663, #19682 ),
 .UNSPECIFIED., .F., .F.,
 ( 4, 3, 3, 3, 3, 3, 3, 3, 3, 3, 3, 3, 3, 3, 3, 3, 3, 3, 3, 3, 3, 3, 3, 3, 3, 3, 3, 3, 3, 3, 3, 3, 3, 3, 3, 3, 3, 3, 3, 3, 3, 3, 3, 3, 3, 3, 3, 3, 3, 3, 3, 3, 3, 3, 3, 3, 3, 3, 3, 3, 3, 3, 3, 3, 3, 3, 3, 3, 3, 3, 4 ),
 ( 0.000000000000000000, 0.01785714285713937630, 0.03571428571428875154, 0.04500001460683692583, 0.05357142857142812437, 0.07142857142856749719, 0.08928571428570687696, 0.1071428571428962584, 0.1100000694613451485, 0.1249999999999956285, 0.1428571428570949986, 0.1607142857142943582, 0.1749999145184668869, 0.1785714285713937421, 0.1964285714285931295, 0.2142857142856925134, 0.2321428571428918730, 0.2400000499947346211, 0.2499999999999912570, 0.2678571428570906132, 0.2857142857142900283, 0.3035714285713893568, 0.3050000289315413227, 0.3214285714285887163, 0.3392857142856881558, 0.3571428571428875154, 0.3699998972919570916, 0.3749999999999868994, 0.3928571428570862833, 0.4107142857142856429, 0.4285714285713849714, 0.4350000984216157995, 0.4464285714285843865, 0.4642857142856838260, 0.4821428571428831300, 0.4999999999999825140, 0.5178571428570818425, 0.5357142857142811465, 0.5535714285713807525, 0.5649999146099302649, 0.5714285714285800566, 0.5892857142856793295, 0.6071428571428788556, 0.6249999999999781286, 0.6300001157399379714, 0.6428571428570775126, 0.6607142857142768166, 0.6785714285713763116, 0.6949999841006686552, 0.6964285714285757267, 0.7142857142856749997, 0.7321428571428744148, 0.7499999999999737987, 0.7599999630366554015, 0.7678571428570730717, 0.7857142857142723757, 0.8035714285713719818, 0.8214285714285712858, 0.8250000985136630716, 0.8392857142856706698, 0.8571428571428700849, 0.8749999999999693578, 0.8899999435708758622, 0.8928571428570687418, 0.9107142857142680459, 0.9285714285713676519, 0.9464285714285669560, 0.9549999984243136009, 0.9642857142856662289, 0.9821428571428657550, 0.9999999999999650280 ),
 .UNSPECIFIED. ) ;
#13262 = ORIENTED_EDGE ( 'NONE', *, *, #6028, .T. ) ;
#13263 = CARTESIAN_POINT ( 'NONE',  ( 1.069380478968006809, 12.49147184623710238, 6.284399451820561033 ) ) ;
#13264 = DIRECTION ( 'NONE',  ( 0.000000000000000000, -1.000000000000000000, -0.000000000000000000 ) ) ;
#13265 = ORIENTED_EDGE ( 'NONE', *, *, #2472, .T. ) ;
#13266 = VECTOR ( 'NONE', #6175, 1000.000000000000000 ) ;
#13267 = CARTESIAN_POINT ( 'NONE',  ( 8.511781261342891369, 21.35551480289056059, -0.1885739448980535138 ) ) ;
#13268 = CYLINDRICAL_SURFACE ( 'NONE', #7159, 0.7950200000000001710 ) ;
#13269 = PLANE ( 'NONE',  #11453 ) ;
#13270 = CYLINDRICAL_SURFACE ( 'NONE', #13981, 30.16250000000000142 ) ;
#13271 = CARTESIAN_POINT ( 'NONE',  ( 1.700472889415836741, 16.44472669448222746, -0.6926365997233963068 ) ) ;
#13272 = ADVANCED_FACE ( 'NONE', ( #1498 ), #4722, .F. ) ;
#13273 = ORIENTED_EDGE ( 'NONE', *, *, #19071, .F. ) ;
#13274 = DIRECTION ( 'NONE',  ( 0.8334497143791944618, 0.000000000000000000, 0.5525953072558966728 ) ) ;
#13275 = CARTESIAN_POINT ( 'NONE',  ( 70.64340948846358970, 1.984375000000000000, -10.93409647675949969 ) ) ;
#13276 = LINE ( 'NONE', #4524, #17015 ) ;
#13277 = CARTESIAN_POINT ( 'NONE',  ( 53.21204579382725797, 37.69740999999999786, -16.58583161195731748 ) ) ;
#13278 = ORIENTED_EDGE ( 'NONE', *, *, #9567, .T. ) ;
#13279 = ORIENTED_EDGE ( 'NONE', *, *, #6461, .F. ) ;
#13280 = CARTESIAN_POINT ( 'NONE',  ( 6.182380192748544445, 11.52015345895104126, 3.309294107830659470 ) ) ;
#13281 = DIRECTION ( 'NONE',  ( 0.000000000000000000, -1.000000000000000000, -0.000000000000000000 ) ) ;
#13282 = ORIENTED_EDGE ( 'NONE', *, *, #4272, .F. ) ;
#13283 = AXIS2_PLACEMENT_3D ( 'NONE', #13755, #12088, #15420 ) ;
#13284 = ORIENTED_EDGE ( 'NONE', *, *, #1564, .F. ) ;
#13285 = DIRECTION ( 'NONE',  ( 0.000000000000000000, 1.000000000000000000, 0.000000000000000000 ) ) ;
#13286 = ORIENTED_EDGE ( 'NONE', *, *, #5349, .T. ) ;
#13287 = CARTESIAN_POINT ( 'NONE',  ( 7.966544624650091500, 11.88367076829663205, 0.8237426769557719686 ) ) ;
#13288 = MANIFOLD_SOLID_BREP ( 'Stock-MAS-676-1', #9572 ) ;
#13289 = CARTESIAN_POINT ( 'NONE',  ( 3.153395120602799917, 17.97939181118854179, 8.120414267292568766 ) ) ;
#13290 = DIRECTION ( 'NONE',  ( 0.000000000000000000, 1.000000000000000000, 0.000000000000000000 ) ) ;
#13291 = CARTESIAN_POINT ( 'NONE',  ( 59.52193197173441774, 34.52875999999999834, -3.260183413611184911 ) ) ;
#13292 = DIRECTION ( 'NONE',  ( 0.000000000000000000, 1.000000000000000000, 0.000000000000000000 ) ) ;
#13293 = DIRECTION ( 'NONE',  ( 0.2490110332224850231, 0.000000000000000000, -0.9685006480810791629 ) ) ;
#13294 = CARTESIAN_POINT ( 'NONE',  ( -0.1894246789259524388, 15.61174044977811803, 0.09809569534440258642 ) ) ;
#13295 = ADVANCED_FACE ( 'NONE', ( #6252 ), #1605, .T. ) ;
#13296 = DIRECTION ( 'NONE',  ( -0.9964481331860213231, 0.000000000000000000, 0.08420877549337203727 ) ) ;
#13297 = ADVANCED_FACE ( 'NONE', ( #21836 ), #2835, .F. ) ;
#13298 = ORIENTED_EDGE ( 'NONE', *, *, #8686, .T. ) ;
#13299 = CARTESIAN_POINT ( 'NONE',  ( 0.7885908350430151925, 19.54577606275120161, 7.374915595215576047 ) ) ;
#13300 = CARTESIAN_POINT ( 'NONE',  ( 59.74839655170352160, -6.356984999999999886, -15.51636860603746193 ) ) ;
#13301 = DIRECTION ( 'NONE',  ( 0.2227372614606430989, 0.000000000000000000, 0.9748785115885020280 ) ) ;
#13302 = CARTESIAN_POINT ( 'NONE',  ( -4.157227781567939928, 9.924415000000001541, 0.1758860224507720060 ) ) ;
#13303 = ORIENTED_EDGE ( 'NONE', *, *, #21261, .F. ) ;
#13304 = CARTESIAN_POINT ( 'NONE',  ( 11.03321510994558352, 12.31537751810604320, -2.946964147034912163 ) ) ;
#13305 = CARTESIAN_POINT ( 'NONE',  ( 21.03437500000000071, 32.54502000000000095, 5.159374999999999822 ) ) ;
#13306 = CARTESIAN_POINT ( 'NONE',  ( 9.091854592231021215, 14.28828935598729011, -3.244019243948331521 ) ) ;
#13307 = EDGE_LOOP ( 'NONE', ( #14292, #20865, #5711, #1372 ) ) ;
#13308 = CARTESIAN_POINT ( 'NONE',  ( 9.171773708691890903, 18.63249697686906714, 7.499116223077195720 ) ) ;
#13309 = LINE ( 'NONE', #4561, #2451 ) ;
#13310 = CARTESIAN_POINT ( 'NONE',  ( 7.199757042754272973, 16.58762552368920851, 7.742064170688478519 ) ) ;
#13311 = CARTESIAN_POINT ( 'NONE',  ( 5.447351731530780228, 1.984375000000000000, 0.8930339070797439494 ) ) ;
#13312 = DIRECTION ( 'NONE',  ( -0.06191955310929833645, 0.000000000000000000, 0.9980811434661738257 ) ) ;
#13313 = VERTEX_POINT ( 'NONE', #21506 ) ;
#13314 = EDGE_CURVE ( 'NONE', #17699, #119, #6362, .T. ) ;
#13315 = CARTESIAN_POINT ( 'NONE',  ( 6.756709577111620568, 20.37078616557504063, -0.1517828402666514531 ) ) ;
#13316 = LINE ( 'NONE', #18370, #21518 ) ;
#13317 = DIRECTION ( 'NONE',  ( -0.000000000000000000, -1.000000000000000000, 0.000000000000000000 ) ) ;
#13318 = EDGE_CURVE ( 'NONE', #6074, #1216, #16968, .T. ) ;
#13319 = DIRECTION ( 'NONE',  ( -0.9724402360367336851, 0.000000000000000000, 0.2331522835762537549 ) ) ;
#13320 = CARTESIAN_POINT ( 'NONE',  ( 6.487363973528258221, 10.93980350523859180, 2.763734740000318268 ) ) ;
#13321 = CARTESIAN_POINT ( 'NONE',  ( 61.65536943582333151, 34.52875999999999834, -11.98363747855214712 ) ) ;
#13322 = CARTESIAN_POINT ( 'NONE',  ( 28.97711086133420366, -42.42568807200000691, -10.71499000000000024 ) ) ;
#13323 = CARTESIAN_POINT ( 'NONE',  ( 21.21496537101402424, -3.671282913444335438, -15.02289707828213139 ) ) ;
#13324 = CARTESIAN_POINT ( 'NONE',  ( -24.20935654380574320, -8.889364999999999739, -25.29247038871795894 ) ) ;
#13325 = ORIENTED_EDGE ( 'NONE', *, *, #17894, .F. ) ;
#13326 = CARTESIAN_POINT ( 'NONE',  ( 8.505511374756364873, 24.59767750000000319, -20.97439202360551747 ) ) ;
#13327 = EDGE_CURVE ( 'NONE', #5503, #2509, #18945, .T. ) ;
#13328 = ORIENTED_EDGE ( 'NONE', *, *, #18775, .F. ) ;
#13329 = CARTESIAN_POINT ( 'NONE',  ( 13.09702908948960598, 13.66552469702472017, 5.688823683958623256 ) ) ;
#13330 = DIRECTION ( 'NONE',  ( -0.3482992169606098365, 0.9330960544336215357, -0.08955115110948595747 ) ) ;
#13331 = AXIS2_PLACEMENT_3D ( 'NONE', #19564, #4529, #11163 ) ;
#13332 = CARTESIAN_POINT ( 'NONE',  ( 11.62339053785985676, -3.109361707316991019, -16.93227153458428447 ) ) ;
#13334 = DIRECTION ( 'NONE',  ( 0.4080888115384288528, 0.000000000000000000, 0.9129422336036122632 ) ) ;
#13333 = CARTESIAN_POINT ( 'NONE',  ( 6.748626741718993571, 18.34719479834194189, 7.834309874210196867 ) ) ;
#13335 = ORIENTED_EDGE ( 'NONE', *, *, #2919, .T. ) ;
#13336 = CARTESIAN_POINT ( 'NONE',  ( -0.2842591080265123304, 20.23672349150513483, 5.180682693245175940 ) ) ;
#13337 = ORIENTED_EDGE ( 'NONE', *, *, #18748, .F. ) ;
#13338 = CARTESIAN_POINT ( 'NONE',  ( 14.05820270259704152, -1.983739999999999393, -15.03781736451272444 ) ) ;
#13339 = EDGE_CURVE ( 'NONE', #21727, #21745, #13670, .T. ) ;
#13340 = EDGE_CURVE ( 'NONE', #5911, #13394, #17082, .T. ) ;
#13341 = ADVANCED_FACE ( 'NONE', ( #1708 ), #16611, .T. ) ;
#13342 = CARTESIAN_POINT ( 'NONE',  ( 11.75011716698597297, -4.547989565168462534, -16.18272918671651084 ) ) ;
#13343 = ORIENTED_EDGE ( 'NONE', *, *, #20903, .T. ) ;
#13344 = CARTESIAN_POINT ( 'NONE',  ( 7.430732595839587340, 16.36411096495813311, -2.221128139217481756 ) ) ;
#13345 = DIRECTION ( 'NONE',  ( 0.000000000000000000, 1.000000000000000000, 0.000000000000000000 ) ) ;
#13346 = CARTESIAN_POINT ( 'NONE',  ( 10.94051986474393523, 19.57796819772926256, 6.737305449978185479 ) ) ;
#13347 = AXIS2_PLACEMENT_3D ( 'NONE', #21178, #4497, #14582 ) ;
#13348 = CARTESIAN_POINT ( 'NONE',  ( 12.14154796308823236, -4.523627393238572658, -16.83224736341038508 ) ) ;
#13349 = ORIENTED_EDGE ( 'NONE', *, *, #13660, .F. ) ;
#13350 = CARTESIAN_POINT ( 'NONE',  ( 10.68002764719964937, 19.26684220934778935, 5.864093243101673458 ) ) ;
#13351 = CARTESIAN_POINT ( 'NONE',  ( 10.64203227393771201, 21.88976505986162024, 0.05508552734995522671 ) ) ;
#13352 = CARTESIAN_POINT ( 'NONE',  ( 38.95864968682538176, -5.166420501038664348, -3.945715010571505310 ) ) ;
#13353 = ORIENTED_EDGE ( 'NONE', *, *, #11526, .F. ) ;
#13354 = EDGE_LOOP ( 'NONE', ( #4150, #3075, #2982, #14912 ) ) ;
#13355 = DIRECTION ( 'NONE',  ( -0.2868778675745011220, 0.000000000000000000, -0.9579671649362034858 ) ) ;
#13357 = DIRECTION ( 'NONE',  ( 0.9790635044817342925, 0.000000000000000000, -0.2035550397114870569 ) ) ;
#13356 = CARTESIAN_POINT ( 'NONE',  ( 4.496700024354473690, 10.96673477554678122, 3.844746723458174031 ) ) ;
#13358 = VERTEX_POINT ( 'NONE', #11998 ) ;
#13359 = CARTESIAN_POINT ( 'NONE',  ( 4.500494465692399082, 20.64052229378682313, 0.7001359311331863955 ) ) ;
#13360 = VERTEX_POINT ( 'NONE', #1927 ) ;
#13361 = AXIS2_PLACEMENT_3D ( 'NONE', #18998, #17361, #15722 ) ;
#13362 = EDGE_LOOP ( 'NONE', ( #89, #16478, #2650, #538 ) ) ;
#13363 = CARTESIAN_POINT ( 'NONE',  ( 0.4297214030689984199, 12.52539863399390541, 3.302885710598653990 ) ) ;
#13364 = EDGE_CURVE ( 'NONE', #9466, #20607, #3708, .T. ) ;
#13365 = DIRECTION ( 'NONE',  ( -0.8583349619704310207, 0.000000000000000000, 0.5130897514657826175 ) ) ;
#13366 = EDGE_LOOP ( 'NONE', ( #15282, #16377, #10263, #21173 ) ) ;
#13367 = CARTESIAN_POINT ( 'NONE',  ( 7.643032390518417429, 21.81816933872264030, 3.222994271250708032 ) ) ;
#13368 = CARTESIAN_POINT ( 'NONE',  ( 4.228318371191494229, 12.14970637543461152, 2.202701631799199866 ) ) ;
#13369 = DIRECTION ( 'NONE',  ( 0.000000000000000000, -1.000000000000000000, 0.000000000000000000 ) ) ;
#13370 = PLANE ( 'NONE',  #15746 ) ;
#13371 = CARTESIAN_POINT ( 'NONE',  ( 2.533239475727145695, 20.31455609140651219, 1.114995646245765748 ) ) ;
#13372 = AXIS2_PLACEMENT_3D ( 'NONE', #3231, #20116, #4989 ) ;
#13373 = ORIENTED_EDGE ( 'NONE', *, *, #3156, .T. ) ;
#13374 = DIRECTION ( 'NONE',  ( 0.000000000000000000, 1.000000000000000000, 0.000000000000000000 ) ) ;
#13375 = DIRECTION ( 'NONE',  ( 0.000000000000000000, -1.000000000000000000, 0.000000000000000000 ) ) ;
#13376 = CARTESIAN_POINT ( 'NONE',  ( 9.828862065001116477, -1.983739999999999393, -16.12522240043857025 ) ) ;
#13377 = ORIENTED_EDGE ( 'NONE', *, *, #18721, .F. ) ;
#13378 = VERTEX_POINT ( 'NONE', #13560 ) ;
#13379 = CARTESIAN_POINT ( 'NONE',  ( 9.244890676200823165, 13.73439867555944716, -2.211585914485044047 ) ) ;
#13380 = CARTESIAN_POINT ( 'NONE',  ( -0.2988811684143778957, 21.11360319320700185, 4.764389704680555226 ) ) ;
#13381 = ORIENTED_EDGE ( 'NONE', *, *, #11385, .T. ) ;
#13382 = ORIENTED_EDGE ( 'NONE', *, *, #21653, .T. ) ;
#13383 = DIRECTION ( 'NONE',  ( 0.8609107660235849613, 0.000000000000000000, -0.5087559856598092844 ) ) ;
#13384 = ORIENTED_EDGE ( 'NONE', *, *, #12657, .T. ) ;
#13385 = CARTESIAN_POINT ( 'NONE',  ( 8.169479316132337132, 11.61242145201585352, 1.724731120145178043 ) ) ;
#13386 = DIRECTION ( 'NONE',  ( 0.9579671649362032637, 0.000000000000000000, -0.2868778675745012885 ) ) ;
#13387 = EDGE_CURVE ( 'NONE', #20548, #20642, #20712, .T. ) ;
#13388 = CARTESIAN_POINT ( 'NONE',  ( 3.164782767117006124, 17.92400674599301880, 8.142467647448141221 ) ) ;
#13389 = CIRCLE ( 'NONE', #6664, 0.3962400000000008138 ) ;
#13390 = FACE_OUTER_BOUND ( 'NONE', #1596, .T. ) ;
#13391 = FACE_OUTER_BOUND ( 'NONE', #12365, .T. ) ;
#13392 = CARTESIAN_POINT ( 'NONE',  ( 0.5982744427495542139, 20.03176192076531947, 1.619753041731076815 ) ) ;
#13393 = DIRECTION ( 'NONE',  ( 0.9790635044817342925, 0.000000000000000000, -0.2035550397114870569 ) ) ;
#13394 = VERTEX_POINT ( 'NONE', #11889 ) ;
#13395 = DIRECTION ( 'NONE',  ( -0.9987059298363656357, 0.000000000000000000, -0.05085730733808393328 ) ) ;
#13396 = FACE_OUTER_BOUND ( 'NONE', #19971, .T. ) ;
#13397 = DIRECTION ( 'NONE',  ( -1.000000000000000000, 0.000000000000000000, 0.000000000000000000 ) ) ;
#13398 = ORIENTED_EDGE ( 'NONE', *, *, #8273, .T. ) ;
#13399 = CARTESIAN_POINT ( 'NONE',  ( 8.135493846614000546, 21.27400681123072346, -0.03209029099654438222 ) ) ;
#13400 = VECTOR ( 'NONE', #8162, 1000.000000000000000 ) ;
#13401 = CARTESIAN_POINT ( 'NONE',  ( 12.97983257214918851, 19.16628937045455316, 6.468072931972185913 ) ) ;
#13402 = VERTEX_POINT ( 'NONE', #3816 ) ;
#13403 = CIRCLE ( 'NONE', #20121, 0.3962400000000008138 ) ;
#13404 = CARTESIAN_POINT ( 'NONE',  ( 6.159189550780465261, 20.31477451228112230, -0.5216155623760124760 ) ) ;
#13405 = CARTESIAN_POINT ( 'NONE',  ( 65.90927232300019512, 30.56064500000000095, -13.30734117861468135 ) ) ;
#13406 = FACE_OUTER_BOUND ( 'NONE', #5641, .T. ) ;
#13407 = CIRCLE ( 'NONE', #8086, 30.16249999999999076 ) ;
#13408 = DIRECTION ( 'NONE',  ( 0.000000000000000000, -1.000000000000000000, 0.000000000000000000 ) ) ;
#13409 = EDGE_CURVE ( 'NONE', #17581, #13937, #1767, .T. ) ;
#13410 = CARTESIAN_POINT ( 'NONE',  ( 50.99913033092320092, 30.56064500000000095, -7.029081061492260751 ) ) ;
#13411 = SHAPE_REPRESENTATION ( 'Pivot Pin', ( #2234 ), #15867 ) ;
#13412 = CARTESIAN_POINT ( 'NONE',  ( 9.830938833968739132, 14.76305577989238138, 7.352198101560677657 ) ) ;
#13413 = PLANE ( 'NONE',  #12361 ) ;
#13414 = DIRECTION ( 'NONE',  ( 0.05085730733808393328, 0.000000000000000000, -0.9987059298363656357 ) ) ;
#13415 = LINE ( 'NONE', #16517, #15287 ) ;
#13416 = AXIS2_PLACEMENT_3D ( 'NONE', #6196, #14512, #11400 ) ;
#13417 = CARTESIAN_POINT ( 'NONE',  ( 4.506322691401866365, 19.87799086262558035, 6.406845734523337832 ) ) ;
#13418 = CARTESIAN_POINT ( 'NONE',  ( 11.97174136233939556, 21.25996874134203551, -17.62449286037261942 ) ) ;
#13419 = CARTESIAN_POINT ( 'NONE',  ( 11.74417331903472395, -6.219808599076323219, -16.98778208059958317 ) ) ;
#13420 = CIRCLE ( 'NONE', #5986, 30.16249999999998721 ) ;
#13421 = FILL_AREA_STYLE_COLOUR ( '', #7463 ) ;
#13422 = ORIENTED_EDGE ( 'NONE', *, *, #13660, .T. ) ;
#13423 = CARTESIAN_POINT ( 'NONE',  ( 10.75023146982646516, 11.88040354724858538, 4.139699607910164225 ) ) ;
#13424 = EDGE_CURVE ( 'NONE', #11296, #5048, #14475, .T. ) ;
#13425 = CARTESIAN_POINT ( 'NONE',  ( -15.61825442841409384, -4.819421976693936571, -10.42024638159965555 ) ) ;
#13426 = CARTESIAN_POINT ( 'NONE',  ( 39.47397446732132664, 38.88803500000000213, 2.793231391354656701 ) ) ;
#13427 = CARTESIAN_POINT ( 'NONE',  ( 12.72388782238154192, 11.86124722755734240, 3.874417171192698017 ) ) ;
#13428 = CARTESIAN_POINT ( 'NONE',  ( -5.536601939709260733, 26.98019749999999917, -30.39452380949970944 ) ) ;
#13429 = CARTESIAN_POINT ( 'NONE',  ( 29.19635173153840313, 1.984375000000000000, -6.218966092919240296 ) ) ;
#13430 = CARTESIAN_POINT ( 'NONE',  ( 19.95088882991241164, -1.593704252466229931, -15.47347923388221425 ) ) ;
#13432 = DIRECTION ( 'NONE',  ( -0.9237641507921654505, 0.000000000000000000, -0.3829618697876189803 ) ) ;
#13431 = CARTESIAN_POINT ( 'NONE',  ( 2.086806850236180733, 20.17421804741920255, 6.415940164516433342 ) ) ;
#13433 = ORIENTED_EDGE ( 'NONE', *, *, #1432, .T. ) ;
#13434 = DIRECTION ( 'NONE',  ( 1.000000000000000000, 0.000000000000000000, 0.000000000000000000 ) ) ;
#13435 = DIRECTION ( 'NONE',  ( 0.2868778675745011220, 0.000000000000000000, 0.9579671649362033747 ) ) ;
#13436 = DIRECTION ( 'NONE',  ( 0.000000000000000000, 1.000000000000000000, 0.000000000000000000 ) ) ;
#13437 = EDGE_CURVE ( 'NONE', #18972, #8773, #8561, .T. ) ;
#13438 = EDGE_CURVE ( 'NONE', #17882, #2409, #20485, .T. ) ;
#13439 = AXIS2_PLACEMENT_3D ( 'NONE', #9412, #1229, #7972 ) ;
#13440 = CARTESIAN_POINT ( 'NONE',  ( 30.78626241496060700, -5.959792500000001603, -2.552201779827368622 ) ) ;
#13441 = VECTOR ( 'NONE', #271, 1000.000000000000000 ) ;
#13442 = CARTESIAN_POINT ( 'NONE',  ( 10.41504388964860084, -3.120051954850537435, -17.35142295629939824 ) ) ;
#13443 = ORIENTED_EDGE ( 'NONE', *, *, #15769, .T. ) ;
#13444 = CARTESIAN_POINT ( 'NONE',  ( 13.05853762340243307, 13.21983372403380130, 5.524725199965593525 ) ) ;
#13445 = CARTESIAN_POINT ( 'NONE',  ( 12.02314496290491874, 11.13213648998272198, 0.7539960825612619377 ) ) ;
#13446 = DIRECTION ( 'NONE',  ( 0.000000000000000000, 1.000000000000000000, 0.000000000000000000 ) ) ;
#13447 = CARTESIAN_POINT ( 'NONE',  ( 7.357671466288501883, 12.62844402333576177, -1.643692759918340851 ) ) ;
#13448 = CARTESIAN_POINT ( 'NONE',  ( 11.87836337660393582, -3.107092027145145874, -16.83199469523789915 ) ) ;
#13449 = DIRECTION ( 'NONE',  ( -0.1132953773954069598, 0.7241889112991808375, -0.6802312681817410667 ) ) ;
#13450 = EDGE_LOOP ( 'NONE', ( #5372, #21841, #8250, #7149 ) ) ;
#13451 = AXIS2_PLACEMENT_3D ( 'NONE', #16559, #1827, #11469 ) ;
#13452 = CARTESIAN_POINT ( 'NONE',  ( 9.775342085382558110, 20.91378398451936960, 3.534348224629963564 ) ) ;
#13453 = CARTESIAN_POINT ( 'NONE',  ( 8.448737300149691265, 21.35108299968154455, -0.1673130223080695478 ) ) ;
#13454 = EDGE_CURVE ( 'NONE', #12175, #2498, #18730, .T. ) ;
#13455 = DIRECTION ( 'NONE',  ( 0.000000000000000000, 1.000000000000000000, 0.000000000000000000 ) ) ;
#13456 = ORIENTED_EDGE ( 'NONE', *, *, #21146, .F. ) ;
#13457 = ORIENTED_EDGE ( 'NONE', *, *, #13636, .F. ) ;
#13458 = PLANE ( 'NONE',  #20844 ) ;
#13459 = CARTESIAN_POINT ( 'NONE',  ( 11.15182637456070580, 12.40253908811542161, -2.879831532321843302 ) ) ;
#13461 = DIRECTION ( 'NONE',  ( 0.000000000000000000, -1.000000000000000000, -6.251883472108000384E-09 ) ) ;
#13460 = CARTESIAN_POINT ( 'NONE',  ( 3.820117857399456973, 19.12888530071778348, -0.7817677823692853467 ) ) ;
#13462 = ORIENTED_EDGE ( 'NONE', *, *, #21733, .T. ) ;
#13463 = CARTESIAN_POINT ( 'NONE',  ( 7.281532115049993870, 18.28463547046064974, 8.039107993424838838 ) ) ;
#13464 = COLOUR_RGB ( '', 0.40784314, 0.44705882, 0.49803922) ;
#13465 = VECTOR ( 'NONE', #1104, 1000.000000000000227 ) ;
#13466 = EDGE_LOOP ( 'NONE', ( #13286, #8072, #11535, #6191 ) ) ;
#13467 = CIRCLE ( 'NONE', #20133, 0.7950200000000003930 ) ;
#13468 = CARTESIAN_POINT ( 'NONE',  ( 1.954387715434429795, 23.81077936178774834, 10.71562499999999929 ) ) ;
#13469 = ORIENTED_EDGE ( 'NONE', *, *, #12211, .T. ) ;
#13470 = DIRECTION ( 'NONE',  ( 0.000000000000000000, 1.000000000000000000, 0.000000000000000000 ) ) ;
#13471 = DIRECTION ( 'NONE',  ( -0.6496772031432439531, 0.000000000000000000, 0.7602101891687401691 ) ) ;
#13472 = CARTESIAN_POINT ( 'NONE',  ( 52.44708915697334106, 34.52875999999999834, 4.020247972991190188 ) ) ;
#13473 = CARTESIAN_POINT ( 'NONE',  ( 2.673620212570479104, 20.58160544162635119, 1.481323531626213663 ) ) ;
#13474 = AXIS2_PLACEMENT_3D ( 'NONE', #1286, #9571, #19632 ) ;
#13475 = VERTEX_POINT ( 'NONE', #5461 ) ;
#13476 = DIRECTION ( 'NONE',  ( 0.3928209820863007851, 0.000000000000000000, -0.9196149607486571176 ) ) ;
#13477 = CARTESIAN_POINT ( 'NONE',  ( 59.65121809612895731, -1.983739999999999837, -2.485718937265306572 ) ) ;
#13478 = DIRECTION ( 'NONE',  ( 0.000000000000000000, -1.000000000000000000, 0.000000000000000000 ) ) ;
#13479 = EDGE_CURVE ( 'NONE', #9714, #21739, #18841, .T. ) ;
#13480 = CARTESIAN_POINT ( 'NONE',  ( 9.907371917564091746, -3.968114999999999615, -13.23786778167655243 ) ) ;
#13481 = LINE ( 'NONE', #20631, #18660 ) ;
#13482 = VERTEX_POINT ( 'NONE', #17187 ) ;
#13483 = ADVANCED_FACE ( 'NONE', ( #8772 ), #15552, .T. ) ;
#13484 = ORIENTED_EDGE ( 'NONE', *, *, #336, .F. ) ;
#13485 = VECTOR ( 'NONE', #17577, 1000.000000000000000 ) ;
#13486 = CARTESIAN_POINT ( 'NONE',  ( 8.438489806275660143, 20.62750485818692070, 0.2245734197965573720 ) ) ;
#13487 = FACE_OUTER_BOUND ( 'NONE', #13466, .T. ) ;
#13488 = EDGE_LOOP ( 'NONE', ( #6844, #13284, #18767, #18090, #15928 ) ) ;
#13489 = ORIENTED_EDGE ( 'NONE', *, *, #20842, .F. ) ;
#13490 = CARTESIAN_POINT ( 'NONE',  ( 28.97711086133420366, -42.42568807200000691, -10.71499000000000024 ) ) ;
#13491 = ORIENTED_EDGE ( 'NONE', *, *, #6432, .T. ) ;
#13492 = CARTESIAN_POINT ( 'NONE',  ( 9.213875215811913932, 16.57205411493795211, 7.219289365333760422 ) ) ;
#13493 = CARTESIAN_POINT ( 'NONE',  ( -15.27766260488554195, -5.953760000000000829, -26.04727837583638461 ) ) ;
#13494 = AXIS2_PLACEMENT_3D ( 'NONE', #4188, #10928, #16358 ) ;
#13495 = VECTOR ( 'NONE', #14640, 1000.000000000000000 ) ;
#13496 = VECTOR ( 'NONE', #5299, 1000.000000000000227 ) ;
#13497 = CARTESIAN_POINT ( 'NONE',  ( 3.428797585246498691, 14.99582101891923180, 8.235017481150693541 ) ) ;
#13498 = VECTOR ( 'NONE', #15802, 1000.000000000000000 ) ;
#13499 = CARTESIAN_POINT ( 'NONE',  ( 49.28028498622276032, 34.52875999999999834, -25.68670502218146368 ) ) ;
#13500 = DIRECTION ( 'NONE',  ( -0.2490110332224846346, 0.000000000000000000, 0.9685006480810792739 ) ) ;
#13501 = LINE ( 'NONE', #20212, #3333 ) ;
#13502 = DIRECTION ( 'NONE',  ( -0.4987171968201975503, 0.000000000000000000, 0.8667647648559581031 ) ) ;
#13503 = CARTESIAN_POINT ( 'NONE',  ( 0.6940729559828254791, 20.23939374610027997, 1.864739730547348096 ) ) ;
#13504 = CARTESIAN_POINT ( 'NONE',  ( -19.99570496368815142, -9.590920198756240467, -10.11526441440630286 ) ) ;
#13505 = ORIENTED_EDGE ( 'NONE', *, *, #16187, .T. ) ;
#13506 = CARTESIAN_POINT ( 'NONE',  ( 0.6866223815748832005, 18.62527059298248489, 1.150325187240316405 ) ) ;
#13507 = CARTESIAN_POINT ( 'NONE',  ( 46.03750000000000142, 32.54502000000000095, -10.31874999999999964 ) ) ;
#13508 = CARTESIAN_POINT ( 'NONE',  ( 53.14266576735293768, -5.167590446840315543, -16.66242751532468702 ) ) ;
#13509 = SURFACE_STYLE_USAGE ( .BOTH. , #3336 ) ;
#13510 = LINE ( 'NONE', #13194, #19366 ) ;
#13511 = CIRCLE ( 'NONE', #19835, 0.5080000000000010063 ) ;
#13512 = ORIENTED_EDGE ( 'NONE', *, *, #16382, .F. ) ;
#13513 = EDGE_CURVE ( 'NONE', #13567, #1356, #20602, .T. ) ;
#13514 = COLOUR_RGB ( '', 0.66274510, 0.83137255, 0.94901961) ;
#13515 = CARTESIAN_POINT ( 'NONE',  ( 11.67896625218249618, 10.41612365926042116, 0.7535808997328219405 ) ) ;
#13516 = LINE ( 'NONE', #12062, #5342 ) ;
#13517 = CARTESIAN_POINT ( 'NONE',  ( 12.66021206568372115, 20.29409823522225054, 5.669750305148447467 ) ) ;
#13518 = ORIENTED_EDGE ( 'NONE', *, *, #15919, .F. ) ;
#13519 = VECTOR ( 'NONE', #4805, 1000.000000000000000 ) ;
#13520 = CARTESIAN_POINT ( 'NONE',  ( 9.447553535191925533, 16.53591467142064175, 7.981982076782735192 ) ) ;
#13521 = AXIS2_PLACEMENT_3D ( 'NONE', #12556, #4140, #10878 ) ;
#13522 = CARTESIAN_POINT ( 'NONE',  ( 1.877778717054381152, 14.88408257588732653, 0.2291485109617275584 ) ) ;
#13523 = CARTESIAN_POINT ( 'NONE',  ( 37.29356535768673098, -6.356984999999999886, -6.700294045292300105 ) ) ;
#13524 = DIRECTION ( 'NONE',  ( -0.9161599507719021540, -0.3242921320961419940, -0.2355537256384720723 ) ) ;
#13525 = CARTESIAN_POINT ( 'NONE',  ( -1.345424459097947834, 20.24316500000000119, 2.648158502653860324 ) ) ;
#13526 = AXIS2_PLACEMENT_3D ( 'NONE', #1577, #14662, #19927 ) ;
#13527 = CARTESIAN_POINT ( 'NONE',  ( 10.28864454875730594, 11.13211821786026157, 0.2008260053232651388 ) ) ;
#13528 = CARTESIAN_POINT ( 'NONE',  ( 1.976491907247917013, 18.25402966388874049, -0.4944100302576455719 ) ) ;
#13529 = LINE ( 'NONE', #5209, #11412 ) ;
#13530 = CIRCLE ( 'NONE', #4359, 30.16250000000000497 ) ;
#13531 = DIRECTION ( 'NONE',  ( -0.8943161143440100380, 0.000000000000000000, -0.4474356798743612806 ) ) ;
#13532 = CARTESIAN_POINT ( 'NONE',  ( 0.1888168487964103914, 20.17819236544972128, 6.192740200012695873 ) ) ;
#13533 = LINE ( 'NONE', #5115, #10603 ) ;
#13534 = DIRECTION ( 'NONE',  ( 0.9685006480810790519, 0.000000000000000000, 0.2490110332224857170 ) ) ;
#13535 = CARTESIAN_POINT ( 'NONE',  ( 12.57351160526011924, -7.145082314903915766, -16.82041929937520663 ) ) ;
#13536 = DIRECTION ( 'NONE',  ( 0.000000000000000000, 1.000000000000000000, -0.000000000000000000 ) ) ;
#13537 = EDGE_CURVE ( 'NONE', #14260, #5609, #9103, .T. ) ;
#13538 = VERTEX_POINT ( 'NONE', #19284 ) ;
#13539 = CARTESIAN_POINT ( 'NONE',  ( 11.14979281629860353, 18.53988176718878478, 7.153212395691411096 ) ) ;
#13540 = CARTESIAN_POINT ( 'NONE',  ( -15.84345693979051894, -5.059254600095735022, -10.46616649349276074 ) ) ;
#13541 = FACE_OUTER_BOUND ( 'NONE', #19666, .T. ) ;
#13542 = CARTESIAN_POINT ( 'NONE',  ( 12.94132309758686716, 17.97498947781735268, 6.146935883453322980 ) ) ;
#13543 = CARTESIAN_POINT ( 'NONE',  ( 11.58844351015046215, -3.109292849304047035, -16.76334073837951877 ) ) ;
#13545 = CARTESIAN_POINT ( 'NONE',  ( 3.805353748838121053, -3.968114999999999615, -22.18284873352824960 ) ) ;
#13544 = CARTESIAN_POINT ( 'NONE',  ( 1.406064764339918005, 15.70174598044015291, 8.911119269253976682 ) ) ;
#13546 = VERTEX_POINT ( 'NONE', #16102 ) ;
#13547 = DIRECTION ( 'NONE',  ( 0.7421532822901569793, 0.000000000000000000, -0.6702301885068642218 ) ) ;
#13548 = LINE ( 'NONE', #7001, #17609 ) ;
#13549 = AXIS2_PLACEMENT_3D ( 'NONE', #5965, #6601, #15033 ) ;
#13550 = CARTESIAN_POINT ( 'NONE',  ( -24.20935654380574320, 41.43438499999999891, -25.29247038871795894 ) ) ;
#13551 = ORIENTED_EDGE ( 'NONE', *, *, #11245, .F. ) ;
#13552 = CARTESIAN_POINT ( 'NONE',  ( 11.98751445987246456, 11.13213648998272198, 0.7646661797260611015 ) ) ;
#13553 = CARTESIAN_POINT ( 'NONE',  ( 3.329379522287787108, 20.49949451679308154, 3.262314715822274724 ) ) ;
#13554 = EDGE_CURVE ( 'NONE', #8439, #14268, #15210, .T. ) ;
#13555 = CIRCLE ( 'NONE', #14629, 2.182812500000000711 ) ;
#13556 = CARTESIAN_POINT ( 'NONE',  ( 11.31768156113191814, 12.85014763714888097, -2.390818890651747353 ) ) ;
#13557 = CARTESIAN_POINT ( 'NONE',  ( 4.619952123971384772, 11.64801722256006045, 1.999733552329578501 ) ) ;
#13558 = CARTESIAN_POINT ( 'NONE',  ( 6.456273409070454328, 10.79806832651256165, 3.236992721971956311 ) ) ;
#13559 = CARTESIAN_POINT ( 'NONE',  ( 13.60955983258148727, -6.467614470005191407, -16.57130822712815998 ) ) ;
#13560 = CARTESIAN_POINT ( 'NONE',  ( 9.828862065001116477, 34.52875999999999834, -16.12522240043857025 ) ) ;
#13561 = EDGE_CURVE ( 'NONE', #13546, #5667, #19388, .T. ) ;
#13562 = ORIENTED_EDGE ( 'NONE', *, *, #11297, .T. ) ;
#13563 = EDGE_CURVE ( 'NONE', #2020, #11999, #708, .T. ) ;
#13564 = CARTESIAN_POINT ( 'NONE',  ( 9.062145815712636221, 21.02807274652383995, 1.621998221968902865 ) ) ;
#13565 = CARTESIAN_POINT ( 'NONE',  ( 10.94235719458289502, 14.15760627606356081, -4.071005994705733322 ) ) ;
#13566 = VECTOR ( 'NONE', #2164, 1000.000000000000114 ) ;
#13567 = VERTEX_POINT ( 'NONE', #21267 ) ;
#13568 = VERTEX_POINT ( 'NONE', #17632 ) ;
#13569 = CYLINDRICAL_SURFACE ( 'NONE', #12343, 1.984375000000000000 ) ;
#13570 = CARTESIAN_POINT ( 'NONE',  ( 11.15697610284867380, 12.37466090015357167, -2.855684010099386771 ) ) ;
#13572 = CARTESIAN_POINT ( 'NONE',  ( 66.03921914090641110, 1.984375000000000000, -11.33033647675950029 ) ) ;
#13571 = CARTESIAN_POINT ( 'NONE',  ( -0.2379154757676318899, 12.59227895038538136, 1.809312566514052145 ) ) ;
#13573 = ORIENTED_EDGE ( 'NONE', *, *, #17344, .T. ) ;
#13574 = CARTESIAN_POINT ( 'NONE',  ( 5.725800361066888833, 21.50854493894243191, 4.016541230030424181 ) ) ;
#13575 = AXIS2_PLACEMENT_3D ( 'NONE', #15495, #9044, #439 ) ;
#13576 = CARTESIAN_POINT ( 'NONE',  ( 44.27024749654656688, 37.69740999999999786, -8.722764363618033201 ) ) ;
#13577 = ORIENTED_EDGE ( 'NONE', *, *, #19455, .F. ) ;
#13578 = CARTESIAN_POINT ( 'NONE',  ( 0.2018155601342993544, 13.25506815275162253, 2.172332146088685079 ) ) ;
#13579 = DIRECTION ( 'NONE',  ( 0.000000000000000000, -1.000000000000000000, -0.000000000000000000 ) ) ;
#13580 = ORIENTED_EDGE ( 'NONE', *, *, #9353, .F. ) ;
#13581 = CIRCLE ( 'NONE', #14656, 9.524999999999996803 ) ;
#13582 = EDGE_CURVE ( 'NONE', #19114, #8118, #5663, .T. ) ;
#13583 = CARTESIAN_POINT ( 'NONE',  ( 3.903363043724838555, 13.16387888568485209, 0.6442466956650357846 ) ) ;
#13584 = FACE_OUTER_BOUND ( 'NONE', #12808, .T. ) ;
#13585 = CARTESIAN_POINT ( 'NONE',  ( 41.78116128337411794, 29.95901653600000003, 7.392073290253172502 ) ) ;
#13586 = VECTOR ( 'NONE', #3245, 1000.000000000000114 ) ;
#13587 = CARTESIAN_POINT ( 'NONE',  ( 66.79943102505561114, -3.968114999999999615, -12.07331878313145168 ) ) ;
#13588 = CARTESIAN_POINT ( 'NONE',  ( 1.788345386425812533, 17.37974145227866885, -0.6040922398381389780 ) ) ;
#13589 = FACE_BOUND ( 'NONE', #20063, .T. ) ;
#13590 = ORIENTED_EDGE ( 'NONE', *, *, #20425, .F. ) ;
#13591 = EDGE_CURVE ( 'NONE', #13313, #1074, #7774, .T. ) ;
#13592 = DIRECTION ( 'NONE',  ( -0.3928209820863022839, 0.000000000000000000, 0.9196149607486564515 ) ) ;
#13593 = CARTESIAN_POINT ( 'NONE',  ( 13.67756757867809725, 12.29391749999999739, 2.571257636385987144 ) ) ;
#13594 = CYLINDRICAL_SURFACE ( 'NONE', #3267, 2.182812499999999378 ) ;
#13595 = CARTESIAN_POINT ( 'NONE',  ( 61.81956123787853130, 34.52875999999999834, -1.238102447480925239 ) ) ;
#13597 = CARTESIAN_POINT ( 'NONE',  ( 19.30248346126309400, -5.034641893688545977, -14.21054282797976498 ) ) ;
#13596 = DIRECTION ( 'NONE',  ( 0.4080888115384288528, 0.000000000000000000, 0.9129422336036122632 ) ) ;
#13598 = ORIENTED_EDGE ( 'NONE', *, *, #7876, .T. ) ;
#13599 = ORIENTED_EDGE ( 'NONE', *, *, #14799, .F. ) ;
#13600 = CARTESIAN_POINT ( 'NONE',  ( 6.737092676267780078, 12.02983150285682079, 4.801046767657766168 ) ) ;
#13602 = CARTESIAN_POINT ( 'NONE',  ( 42.92377690484065056, 0.000000000000000000, 4.437564921049077071 ) ) ;
#13601 = CARTESIAN_POINT ( 'NONE',  ( 5.035740336155781982, 11.34978398626420137, 5.613186140933690282 ) ) ;
#13603 = AXIS2_PLACEMENT_3D ( 'NONE', #12651, #10773, #4243 ) ;
#13604 = ORIENTED_EDGE ( 'NONE', *, *, #20038, .F. ) ;
#13605 = ORIENTED_EDGE ( 'NONE', *, *, #83, .F. ) ;
#13606 = DIRECTION ( 'NONE',  ( 0.4210968886563865587, 0.9005306316452192927, 0.1082681478209225612 ) ) ;
#13607 = ORIENTED_EDGE ( 'NONE', *, *, #18883, .T. ) ;
#13608 = CARTESIAN_POINT ( 'NONE',  ( 9.137988923863366253, 13.24564614376286187, 6.127326076054989912 ) ) ;
#13609 = VECTOR ( 'NONE', #11725, 1000.000000000000114 ) ;
#13610 = CARTESIAN_POINT ( 'NONE',  ( 3.366847080470771747, 13.90270457291361161, 7.709217921812351548 ) ) ;
#13611 = ADVANCED_FACE ( 'NONE', ( #21154 ), #7458, .F. ) ;
#13612 = ADVANCED_FACE ( 'NONE', ( #19053 ), #3930, .F. ) ;
#13613 = EDGE_CURVE ( 'NONE', #107, #21520, #2479, .T. ) ;
#13614 = CARTESIAN_POINT ( 'NONE',  ( 11.42842559562532578, 36.51313500000000545, 1.673196738795719174 ) ) ;
#13615 = DIRECTION ( 'NONE',  ( 0.2490110332224846623, 0.000000000000000000, -0.9685006480810793850 ) ) ;
#13616 = CARTESIAN_POINT ( 'NONE',  ( -0.1883589726742697090, 15.66015328560438391, 0.09064164159222751205 ) ) ;
#13617 = FACE_BOUND ( 'NONE', #6218, .T. ) ;
#13618 = ORIENTED_EDGE ( 'NONE', *, *, #13454, .F. ) ;
#13619 = CARTESIAN_POINT ( 'NONE',  ( 5.049881630641887220, 18.75692939610809162, 7.401303026328372781 ) ) ;
#13620 = DIRECTION ( 'NONE',  ( 0.6702301885068628895, 0.000000000000000000, 0.7421532822901579785 ) ) ;
#13621 = CARTESIAN_POINT ( 'NONE',  ( 52.36700307908941454, -6.956221690221880749, -17.43679683612511155 ) ) ;
#13622 = CARTESIAN_POINT ( 'NONE',  ( 12.91596452321051558, 19.43893749999999798, 2.799331278665067479 ) ) ;
#13623 = VERTEX_POINT ( 'NONE', #14437 ) ;
#13624 = CARTESIAN_POINT ( 'NONE',  ( 14.14253296582467634, 21.25787525723532312, 4.279652095381059063 ) ) ;
#13625 = LINE ( 'NONE', #16721, #8879 ) ;
#13626 = CARTESIAN_POINT ( 'NONE',  ( 10.81036398341225713, 21.91646156000656021, 0.6078543174893448198 ) ) ;
#13627 = EDGE_LOOP ( 'NONE', ( #15832, #6792, #10613, #14672, #663, #16607 ) ) ;
#13628 = ORIENTED_EDGE ( 'NONE', *, *, #17995, .T. ) ;
#13629 = DIRECTION ( 'NONE',  ( 1.000000000000000000, 0.000000000000000000, 0.000000000000000000 ) ) ;
#13630 = CARTESIAN_POINT ( 'NONE',  ( 8.177763578858511906, 10.79888309947691205, 1.796606758151653604 ) ) ;
#13631 = CARTESIAN_POINT ( 'NONE',  ( 2.400718128888100544, 20.09598732912352403, 6.282947492075177998 ) ) ;
#13632 = DIRECTION ( 'NONE',  ( 0.000000000000000000, -1.000000000000000000, 0.000000000000000000 ) ) ;
#13633 = CYLINDRICAL_SURFACE ( 'NONE', #18365, 0.7950200000000003930 ) ;
#13634 = CARTESIAN_POINT ( 'NONE',  ( -46.55773479047372376, 43.41875999999999891, -7.870535429687039120 ) ) ;
#13635 = VECTOR ( 'NONE', #133, 1000.000000000000000 ) ;
#13636 = EDGE_CURVE ( 'NONE', #9339, #4938, #10950, .T. ) ;
#13637 = DIRECTION ( 'NONE',  ( -0.9579671649362032637, -2.486588751566399063E-16, 0.2868778675745010664 ) ) ;
#13638 = CARTESIAN_POINT ( 'NONE',  ( 6.902807237671314766, 11.20245161629656039, 3.097827888567519228 ) ) ;
#13639 = CARTESIAN_POINT ( 'NONE',  ( 5.318830492975814117, 13.90914350924470000, 7.343574724398199471 ) ) ;
#13640 = CARTESIAN_POINT ( 'NONE',  ( 4.000918489741002837, 19.12888530071778348, -0.8359112872416241125 ) ) ;
#13641 = DIRECTION ( 'NONE',  ( -1.000000000000000000, 0.000000000000000000, 0.000000000000000000 ) ) ;
#13642 = CARTESIAN_POINT ( 'NONE',  ( 20.24471977733230332, -1.311003557817993492, -14.75211372363476414 ) ) ;
#13643 = CARTESIAN_POINT ( 'NONE',  ( 5.229160492742135347, 17.31893540436420764, 8.031536564559639046 ) ) ;
#13644 = CARTESIAN_POINT ( 'NONE',  ( 17.02725982432203367, 36.51313500000000545, -14.27444360421403857 ) ) ;
#13645 = DIRECTION ( 'NONE',  ( 0.2490110332224850509, 0.000000000000000000, -0.9685006480810792739 ) ) ;
#13646 = CARTESIAN_POINT ( 'NONE',  ( 13.96963285379384878, -8.018802334511677898, -16.52276729540345457 ) ) ;
#13647 = LINE ( 'NONE', #10194, #19081 ) ;
#13648 = CARTESIAN_POINT ( 'NONE',  ( 9.093866485257809273, 21.83689553850923204, 1.689583340911293030 ) ) ;
#13649 = CARTESIAN_POINT ( 'NONE',  ( 32.52436584422698473, -1.983739999999999837, 1.884807767196291284 ) ) ;
#13650 = ORIENTED_EDGE ( 'NONE', *, *, #7092, .F. ) ;
#13651 = CARTESIAN_POINT ( 'NONE',  ( 12.84502056709592033, 18.48422115218343009, 5.947007296923204400 ) ) ;
#13652 = CARTESIAN_POINT ( 'NONE',  ( 17.21369304301024172, -7.336514211874763269, -15.87346308029872333 ) ) ;
#13653 = LINE ( 'NONE', #21818, #14495 ) ;
#13654 = VERTEX_POINT ( 'NONE', #604 ) ;
#13655 = SHAPE_DEFINITION_REPRESENTATION ( #11454, #21464 ) ;
#13656 = CARTESIAN_POINT ( 'NONE',  ( -2.028188046367890074, 22.62314500000000095, 0.3682158094503220069 ) ) ;
#13657 = CARTESIAN_POINT ( 'NONE',  ( 4.584455248502485425, 19.89944416103447367, 1.015146957114681614 ) ) ;
#13658 = DIRECTION ( 'NONE',  ( 1.000000000000000000, 0.000000000000000000, 0.000000000000000000 ) ) ;
#13659 = DIRECTION ( 'NONE',  ( 0.000000000000000000, 1.000000000000000000, 0.000000000000000000 ) ) ;
#13660 = EDGE_CURVE ( 'NONE', #18734, #17581, #7349, .T. ) ;
#13661 = CARTESIAN_POINT ( 'NONE',  ( 17.36102099471316507, 2.301167714194472413, -15.54280354277228682 ) ) ;
#13662 = VERTEX_POINT ( 'NONE', #12662 ) ;
#13663 = CARTESIAN_POINT ( 'NONE',  ( 6.701167270133946197, 11.82549305421424179, 4.285450746564428037 ) ) ;
#13664 = CARTESIAN_POINT ( 'NONE',  ( 3.783379877289300364, 20.55809296471286629, 4.452500340783561938 ) ) ;
#13665 = CARTESIAN_POINT ( 'NONE',  ( 10.71277408803009124, 11.64784025693482228, 3.874468920058604215 ) ) ;
#13666 = CARTESIAN_POINT ( 'NONE',  ( 7.591282571684015323, 18.34719479834194189, 7.581963743311560755 ) ) ;
#13667 = CARTESIAN_POINT ( 'NONE',  ( 11.28984340714546697, 17.71682859275886557, 7.541597259675597797 ) ) ;
#13668 = CARTESIAN_POINT ( 'NONE',  ( 42.94469661997857912, -76.79125307200000350, -18.48251861828712705 ) ) ;
#13669 = CARTESIAN_POINT ( 'NONE',  ( 11.88276372161184113, -2.817112673463340933, -16.81723252566703053 ) ) ;
#13670 = LINE ( 'NONE', #500, #357 ) ;
#13671 = EDGE_CURVE ( 'NONE', #1117, #16563, #2375, .T. ) ;
#13672 = AXIS2_PLACEMENT_3D ( 'NONE', #4477, #18185, #13004 ) ;
#13673 = ORIENTED_EDGE ( 'NONE', *, *, #19487, .F. ) ;
#13674 = CARTESIAN_POINT ( 'NONE',  ( 9.882382622271025596, 20.81632985100941013, 3.819104690091920329 ) ) ;
#13675 = CARTESIAN_POINT ( 'NONE',  ( 10.33786395622847820, 10.45470314796870248, 2.195665064187855897 ) ) ;
#13676 = ORIENTED_EDGE ( 'NONE', *, *, #20457, .F. ) ;
#13677 = DIRECTION ( 'NONE',  ( -0.2490110332224850509, 0.000000000000000000, 0.9685006480810792739 ) ) ;
#13678 = CARTESIAN_POINT ( 'NONE',  ( 42.66304184606194383, 32.54502000000000095, -19.22597499813143784 ) ) ;
#13680 = DIRECTION ( 'NONE',  ( -0.9790635044817342925, 0.000000000000000000, 0.2035550397114870846 ) ) ;
#13679 = CARTESIAN_POINT ( 'NONE',  ( 3.278096675365355317, 13.69792732696330262, -0.6529983330018749310 ) ) ;
#13681 = VERTEX_POINT ( 'NONE', #9331 ) ;
#13682 = CARTESIAN_POINT ( 'NONE',  ( 7.136194838460433232, 11.81701620255667606, 6.040694753304580722 ) ) ;
#13683 = LINE ( 'NONE', #20279, #2410 ) ;
#13684 = ORIENTED_EDGE ( 'NONE', *, *, #1288, .T. ) ;
#13685 = EDGE_CURVE ( 'NONE', #18743, #16186, #5689, .T. ) ;
#13686 = AXIS2_PLACEMENT_3D ( 'NONE', #12475, #2508, #19529 ) ;
#13687 = LINE ( 'NONE', #18745, #2605 ) ;
#13688 = EDGE_LOOP ( 'NONE', ( #16995, #5958, #19633, #13791 ) ) ;
#13689 = ADVANCED_FACE ( 'NONE', ( #6009 ), #17528, .F. ) ;
#13690 = CARTESIAN_POINT ( 'NONE',  ( 3.773036282072748993, 14.18962759126609186, -0.1098811704971767444 ) ) ;
#13691 = DIRECTION ( 'NONE',  ( 0.000000000000000000, 1.000000000000000000, 0.000000000000000000 ) ) ;
#13692 = LINE ( 'NONE', #18637, #13087 ) ;
#13693 = FACE_OUTER_BOUND ( 'NONE', #16051, .T. ) ;
#13694 = CARTESIAN_POINT ( 'NONE',  ( 3.049180314527587310, 21.09804464240151134, 2.479317242939253596 ) ) ;
#13695 = CARTESIAN_POINT ( 'NONE',  ( 1.786785375309217994, 8.953154907895765291, 10.71397434136291693 ) ) ;
#13696 = ORIENTED_EDGE ( 'NONE', *, *, #20646, .F. ) ;
#13697 = DIRECTION ( 'NONE',  ( 0.000000000000000000, 1.000000000000000000, 0.000000000000000000 ) ) ;
#13698 = CARTESIAN_POINT ( 'NONE',  ( -23.01875000000000071, 0.000000000000000000, -3.968750000000000000 ) ) ;
#13699 = LINE ( 'NONE', #1958, #9491 ) ;
#13701 = CARTESIAN_POINT ( 'NONE',  ( 15.97178949557365790, -7.235176167653088797, -14.86884501417147320 ) ) ;
#13700 = CARTESIAN_POINT ( 'NONE',  ( -3.042350287543033716, 2.373947500000000765, -26.17378113315171007 ) ) ;
#13702 = VERTEX_POINT ( 'NONE', #4367 ) ;
#13703 = ORIENTED_EDGE ( 'NONE', *, *, #10758, .F. ) ;
#13704 = CARTESIAN_POINT ( 'NONE',  ( 11.14922546541893489, 15.75027095350177397, 6.909280940405325033 ) ) ;
#13705 = VECTOR ( 'NONE', #13955, 1000.000000000000000 ) ;
#13707 = DIRECTION ( 'NONE',  ( -0.000000000000000000, -1.000000000000000000, 0.000000000000000000 ) ) ;
#13706 = CARTESIAN_POINT ( 'NONE',  ( 7.600020092372349545, 14.71802924512825683, 8.258015545363242893 ) ) ;
#13708 = EDGE_LOOP ( 'NONE', ( #15266, #11714, #12792, #6489 ) ) ;
#13709 = EDGE_CURVE ( 'NONE', #12389, #736, #11104, .T. ) ;
#13710 = EDGE_LOOP ( 'NONE', ( #16472, #17475, #4620, #8732, #14372, #9104 ) ) ;
#13711 = DIRECTION ( 'NONE',  ( -0.06191955310929838502, 0.000000000000000000, 0.9980811434661737147 ) ) ;
#13712 = VERTEX_POINT ( 'NONE', #19174 ) ;
#13713 = CARTESIAN_POINT ( 'NONE',  ( 7.457035429875517707, 14.48312770791961235, -1.753970211364317633 ) ) ;
#13714 = CARTESIAN_POINT ( 'NONE',  ( 46.03750000000000142, -3.968114999999999615, -10.31874999999999964 ) ) ;
#13715 = ADVANCED_FACE ( 'NONE', ( #14548 ), #4037, .F. ) ;
#13716 = ORIENTED_EDGE ( 'NONE', *, *, #12819, .T. ) ;
#13717 = EDGE_CURVE ( 'NONE', #21414, #17151, #21196, .T. ) ;
#13718 = CARTESIAN_POINT ( 'NONE',  ( 3.422385042412149136, 14.70423030993896774, 8.132674026271640599 ) ) ;
#13719 = AXIS2_PLACEMENT_3D ( 'NONE', #8, #18582, #8736 ) ;
#13720 = CARTESIAN_POINT ( 'NONE',  ( 47.80475250345343596, -6.356985000000002550, -11.91473563638196786 ) ) ;
#13721 = CARTESIAN_POINT ( 'NONE',  ( 65.47912282493159353, 0.000000000000000000, -13.30734117861468135 ) ) ;
#13722 = CARTESIAN_POINT ( 'NONE',  ( -0.1410424437649658302, 13.95926234754164597, 0.6541928679012153358 ) ) ;
#13723 = FACE_OUTER_BOUND ( 'NONE', #10924, .T. ) ;
#13724 = ORIENTED_EDGE ( 'NONE', *, *, #16092, .T. ) ;
#13725 = AXIS2_PLACEMENT_3D ( 'NONE', #18501, #20145, #5020 ) ;
#13726 = CARTESIAN_POINT ( 'NONE',  ( -49.72082486877479113, -5.714364999999999029, -7.603226040068017610 ) ) ;
#13727 = CARTESIAN_POINT ( 'NONE',  ( 56.91751438644678984, 0.000000000000000000, -20.96198986413465448 ) ) ;
#13728 = DIRECTION ( 'NONE',  ( -0.9579671649362032637, 0.000000000000000000, 0.2868778675745010664 ) ) ;
#13729 = ORIENTED_EDGE ( 'NONE', *, *, #14952, .F. ) ;
#13730 = CARTESIAN_POINT ( 'NONE',  ( 10.01244073014268920, 10.54134736952624252, 2.290216055019587138 ) ) ;
#13731 = FACE_OUTER_BOUND ( 'NONE', #4815, .T. ) ;
#13732 = CARTESIAN_POINT ( 'NONE',  ( 12.07419610447281144, 21.48700711848800182, 4.104121981384611040 ) ) ;
#13733 = EDGE_LOOP ( 'NONE', ( #21190, #6013, #20267, #14586 ) ) ;
#13734 = EDGE_CURVE ( 'NONE', #2204, #6613, #1354, .T. ) ;
#13735 = ORIENTED_EDGE ( 'NONE', *, *, #4790, .T. ) ;
#13736 = EDGE_CURVE ( 'NONE', #18192, #6074, #9203, .T. ) ;
#13737 = CARTESIAN_POINT ( 'NONE',  ( 23.91535545868163126, 23.75961143032650114, -3.395287945660274254 ) ) ;
#13738 = ADVANCED_FACE ( 'NONE', ( #16523 ), #7892, .T. ) ;
#13739 = VECTOR ( 'NONE', #6423, 1000.000000000000000 ) ;
#13740 = CARTESIAN_POINT ( 'NONE',  ( 9.493382606263734758, 14.90386241890908181, 7.804904356304905200 ) ) ;
#13741 = CARTESIAN_POINT ( 'NONE',  ( 0.2231702038951091094, 13.13563057234646081, 2.167777268876749819 ) ) ;
#13742 = CARTESIAN_POINT ( 'NONE',  ( 6.123273286415696681, 11.97223630154925722, 1.629447004418834055 ) ) ;
#13743 = CARTESIAN_POINT ( 'NONE',  ( 1.256988000113886894, 20.19907556228512391, 3.394663028293312568 ) ) ;
#13744 = DIRECTION ( 'NONE',  ( -0.08420877549337300871, 0.000000000000000000, -0.9964481331860212121 ) ) ;
#13745 = VECTOR ( 'NONE', #19038, 1000.000000000000000 ) ;
#13746 = CARTESIAN_POINT ( 'NONE',  ( 9.794783782024321539, 14.67110634242510159, 7.680502800501443517 ) ) ;
#13747 = CARTESIAN_POINT ( 'NONE',  ( 5.342884009753714025, 14.20367987736782034, 7.509086329562091322 ) ) ;
#13748 = CARTESIAN_POINT ( 'NONE',  ( 31.68988926855799448, 32.54502000000000095, 1.626235259850384418 ) ) ;
#13749 = CARTESIAN_POINT ( 'NONE',  ( 4.478280779456667027, 20.54582653591270258, 0.3636022304821014961 ) ) ;
#13750 = CARTESIAN_POINT ( 'NONE',  ( 13.67756757867809725, 30.54508749999999750, 2.571257636385987144 ) ) ;
#13751 = CIRCLE ( 'NONE', #4555, 0.7950200000000000600 ) ;
#13752 = CARTESIAN_POINT ( 'NONE',  ( 8.011380105705496746, -1.594802499999999013, -19.05252355006962617 ) ) ;
#13753 = CARTESIAN_POINT ( 'NONE',  ( 0.7860029000012983547, 19.67029402086490109, 2.268881696640435042 ) ) ;
#13754 = CARTESIAN_POINT ( 'NONE',  ( 1.952969610814715207, 23.80837275291289856, 8.731249999999999289 ) ) ;
#13755 = CARTESIAN_POINT ( 'NONE',  ( 66.03921914090641110, 0.000000000000000000, -11.33033647675950029 ) ) ;
#13756 = CARTESIAN_POINT ( 'NONE',  ( 12.80420541122094846, -7.335296459352831810, -16.77213161543806308 ) ) ;
#13757 = FACE_OUTER_BOUND ( 'NONE', #19985, .T. ) ;
#13758 = CARTESIAN_POINT ( 'NONE',  ( 8.775219136977288059, 21.64129978188946168, 0.8126495212682610658 ) ) ;
#13759 = CARTESIAN_POINT ( 'NONE',  ( 26.59062499999999929, 1.984057500000000251, 10.71562499999999929 ) ) ;
#13760 = ADVANCED_FACE ( 'NONE', ( #9545 ), #14992, .T. ) ;
#13761 = EDGE_LOOP ( 'NONE', ( #16771, #18641, #5072, #5381, #3914, #20619, #4748, #1395, #19339, #1040, #3139, #15348, #20733, #11716, #8685, #14621, #17734, #6127, #198, #632, #20977 ) ) ;
#13762 = ADVANCED_FACE ( 'NONE', ( #19820 ), #13220, .T. ) ;
#13763 = CARTESIAN_POINT ( 'NONE',  ( 12.37075837638908915, 11.27712503541973277, 2.326519893733080657 ) ) ;
#13764 = CARTESIAN_POINT ( 'NONE',  ( 11.76154713882772995, -4.503972587472946820, -15.73284477506779133 ) ) ;
#13766 = DIRECTION ( 'NONE',  ( -0.3482992169606098365, 0.9330960544336215357, -0.08955115110948595747 ) ) ;
#13765 = CARTESIAN_POINT ( 'NONE',  ( 3.125990652992958641, 16.48662853297853914, 8.702465120992709302 ) ) ;
#13767 = VERTEX_POINT ( 'NONE', #9859 ) ;
#13768 = SHAPE_DEFINITION_REPRESENTATION ( #12499, #11147 ) ;
#13769 = CYLINDRICAL_SURFACE ( 'NONE', #5938, 1.190624999999999378 ) ;
#13770 = CARTESIAN_POINT ( 'NONE',  ( 6.118335074779962746, 11.59259103338027153, 2.921910985984132125 ) ) ;
#13771 = ORIENTED_EDGE ( 'NONE', *, *, #17786, .T. ) ;
#13772 = CARTESIAN_POINT ( 'NONE',  ( 8.005991736905883727, 19.55876953988840228, -1.089244621163904192 ) ) ;
#13773 = AXIS2_PLACEMENT_3D ( 'NONE', #11174, #14630, #9403 ) ;
#13774 = CARTESIAN_POINT ( 'NONE',  ( 8.949934402927555155, 12.18626401121546188, 5.089483566546638471 ) ) ;
#13775 = CARTESIAN_POINT ( 'NONE',  ( 3.985841724706598921, 14.84625823140281753, 8.562040005760753303 ) ) ;
#13776 = CARTESIAN_POINT ( 'NONE',  ( 12.90414695137542367, 11.26929059074382167, 4.646971329330398248 ) ) ;
#13777 = FACE_OUTER_BOUND ( 'NONE', #15818, .T. ) ;
#13778 = CARTESIAN_POINT ( 'NONE',  ( 18.19593279813170028, 0.2866705963667399715, -14.77465059166826578 ) ) ;
#13779 = DIRECTION ( 'NONE',  ( 0.000000000000000000, 1.000000000000000000, 0.000000000000000000 ) ) ;
#13780 = CIRCLE ( 'NONE', #4241, 3.175000000000000711 ) ;
#13781 = ORIENTED_EDGE ( 'NONE', *, *, #19723, .T. ) ;
#13782 = CARTESIAN_POINT ( 'NONE',  ( 12.49492969781971397, 10.42866963796318025, 2.723955664945219013 ) ) ;
#13783 = EDGE_LOOP ( 'NONE', ( #18013, #20641, #12602, #17669, #20108, #19074, #17677, #7663 ) ) ;
#13784 = ADVANCED_FACE ( 'NONE', ( #1152 ), #3035, .T. ) ;
#13785 = CARTESIAN_POINT ( 'NONE',  ( 10.27191476923467839, 11.36650105605588124, 2.042190157982642695 ) ) ;
#13786 = CARTESIAN_POINT ( 'NONE',  ( 13.28822531734660828, 34.52875999999999834, -15.23578611614444078 ) ) ;
#13787 = DIRECTION ( 'NONE',  ( -0.9790635044817342925, 0.000000000000000000, 0.2035550397114870846 ) ) ;
#13788 = AXIS2_PLACEMENT_3D ( 'NONE', #1362, #9728, #19579 ) ;
#13790 = CARTESIAN_POINT ( 'NONE',  ( 18.25624999999999787, 16.27314499999999953, 10.71562499999999929 ) ) ;
#13789 = CARTESIAN_POINT ( 'NONE',  ( 4.105856576153292359, 20.47280481670116359, 0.5329862511081018273 ) ) ;
#13791 = ORIENTED_EDGE ( 'NONE', *, *, #21666, .F. ) ;
#13792 = CARTESIAN_POINT ( 'NONE',  ( 7.511152631442144845, 14.04345836577225093, 7.903093247502026131 ) ) ;
#13793 = CIRCLE ( 'NONE', #19412, 0.3962400000000000366 ) ;
#13794 = LINE ( 'NONE', #13576, #11590 ) ;
#13795 = VERTEX_POINT ( 'NONE', #21708 ) ;
#13796 = B_SPLINE_CURVE_WITH_KNOTS ( 'NONE', 3,
 ( #12606, #12393, #769, #20546, #8834 ),
 .UNSPECIFIED., .F., .F.,
 ( 4, 1, 4 ),
 ( 0.5007142149769521211, 0.7499992869954825725, 1.000000000000000000 ),
 .UNSPECIFIED. ) ;
#13797 = CIRCLE ( 'NONE', #6010, 30.16249999999998721 ) ;
#13798 = DIRECTION ( 'NONE',  ( 0.08420877549337300871, 0.000000000000000000, 0.9964481331860212121 ) ) ;
#13799 = EDGE_LOOP ( 'NONE', ( #15813, #13512, #14414, #5695 ) ) ;
#13800 = CARTESIAN_POINT ( 'NONE',  ( 38.23013820809905638, 0.000000000000000000, -14.22485453658974031 ) ) ;
#13801 = FACE_OUTER_BOUND ( 'NONE', #12652, .T. ) ;
#13802 = VECTOR ( 'NONE', #21477, 1000.000000000000000 ) ;
#13803 = DIRECTION ( 'NONE',  ( 0.6702301885068628895, 0.000000000000000000, 0.7421532822901579785 ) ) ;
#13804 = CARTESIAN_POINT ( 'NONE',  ( 5.183650323967657236, 18.93835688769866010, 8.121491601508173730 ) ) ;
#13805 = CARTESIAN_POINT ( 'NONE',  ( 30.78626241496060700, 30.50833916023545811, -2.552201779827368622 ) ) ;
#13806 = VERTEX_POINT ( 'NONE', #1470 ) ;
#13807 = DIRECTION ( 'NONE',  ( -0.08420877549337300871, 0.000000000000000000, -0.9964481331860212121 ) ) ;
#13808 = CYLINDRICAL_SURFACE ( 'NONE', #2184, 9.524999999999996803 ) ;
#13809 = CARTESIAN_POINT ( 'NONE',  ( 1.581041518826207692, -14.84248999999999974, -20.30277549736237575 ) ) ;
#13810 = CARTESIAN_POINT ( 'NONE',  ( 20.76310168089343478, -1.983739999999999393, -11.26763008640078212 ) ) ;
#13812 = CARTESIAN_POINT ( 'NONE',  ( 16.21443133523606406, -7.210654292967314305, -14.81810956799547974 ) ) ;
#13811 = DIRECTION ( 'NONE',  ( 0.9173788132826626862, 0.000000000000000000, -0.3980152169705242216 ) ) ;
#13813 = ORIENTED_EDGE ( 'NONE', *, *, #12771, .F. ) ;
#13814 = VERTEX_POINT ( 'NONE', #21594 ) ;
#13815 = EDGE_CURVE ( 'NONE', #699, #1968, #9985, .T. ) ;
#13816 = CARTESIAN_POINT ( 'NONE',  ( 8.534517951019410020, 19.62664610146546096, 6.068736627783791526 ) ) ;
#13817 = CIRCLE ( 'NONE', #17684, 3.968750000000000000 ) ;
#13819 = CARTESIAN_POINT ( 'NONE',  ( 59.65121809612895731, 0.000000000000000000, -2.485718937265306572 ) ) ;
#13818 = CARTESIAN_POINT ( 'NONE',  ( 5.894278812470819418, 11.58534598419692152, 0.5893802728092781829 ) ) ;
#13820 = VERTEX_POINT ( 'NONE', #11438 ) ;
#13821 = CARTESIAN_POINT ( 'NONE',  ( 5.398353993155480701, 12.72011693706338242, 7.404239398001607242 ) ) ;
#13822 = ORIENTED_EDGE ( 'NONE', *, *, #20904, .T. ) ;
#13823 = DIRECTION ( 'NONE',  ( 0.000000000000000000, 1.000000000000000000, 0.000000000000000000 ) ) ;
#13824 = ORIENTED_EDGE ( 'NONE', *, *, #17671, .T. ) ;
#13825 = AXIS2_PLACEMENT_3D ( 'NONE', #17841, #10761, #7328 ) ;
#13826 = CARTESIAN_POINT ( 'NONE',  ( 7.793721086304733703, 18.58975311028322963, -1.609092735773066440 ) ) ;
#13827 = ORIENTED_EDGE ( 'NONE', *, *, #13166, .T. ) ;
#13828 = CIRCLE ( 'NONE', #397, 1.191259999999999097 ) ;
#13829 = AXIS2_PLACEMENT_3D ( 'NONE', #6591, #18413, #5665 ) ;
#13830 = AXIS2_PLACEMENT_3D ( 'NONE', #21164, #7359, #9113 ) ;
#13831 = EDGE_CURVE ( 'NONE', #21627, #5959, #12040, .T. ) ;
#13832 = CARTESIAN_POINT ( 'NONE',  ( 8.505511374756364873, 6.343967500000000648, -20.97439202360551747 ) ) ;
#13833 = CARTESIAN_POINT ( 'NONE',  ( -17.46249999999999858, -1.587500000000002132, 0.000000000000000000 ) ) ;
#13834 = CARTESIAN_POINT ( 'NONE',  ( 2.981856859474616872, 19.70546197453703030, 7.926161949011188312 ) ) ;
#13835 = FACE_BOUND ( 'NONE', #15897, .T. ) ;
#13836 = EDGE_LOOP ( 'NONE', ( #10052, #6069, #14686, #16494 ) ) ;
#13837 = CARTESIAN_POINT ( 'NONE',  ( 5.143049725565362884, 20.63862493749866189, 2.188920118661080938 ) ) ;
#13838 = DIRECTION ( 'NONE',  ( 0.2868778675745011220, 0.000000000000000000, 0.9579671649362033747 ) ) ;
#13839 = CARTESIAN_POINT ( 'NONE',  ( 53.25054008256628180, -5.160457323442601663, -16.54160408289469686 ) ) ;
#13840 = CARTESIAN_POINT ( 'NONE',  ( 62.90077106633562209, -14.84248999999999974, 8.141649473166729933 ) ) ;
#13841 = VECTOR ( 'NONE', #4553, 1000.000000000000000 ) ;
#13842 = VERTEX_POINT ( 'NONE', #8324 ) ;
#13843 = EDGE_CURVE ( 'NONE', #10772, #19175, #7082, .T. ) ;
#13844 = CARTESIAN_POINT ( 'NONE',  ( 9.540165638950465876, 10.83116634084218077, 0.3186190329235050744 ) ) ;
#13845 = EDGE_CURVE ( 'NONE', #14616, #831, #18182, .T. ) ;
#13846 = EDGE_CURVE ( 'NONE', #19005, #17300, #15224, .T. ) ;
#13847 = DIRECTION ( 'NONE',  ( -0.9964481331860213231, 0.000000000000000000, 0.08420877549337311974 ) ) ;
#13848 = CARTESIAN_POINT ( 'NONE',  ( 12.26704403196416848, 21.18870809390503140, 4.628066114304389522 ) ) ;
#13849 = VERTEX_POINT ( 'NONE', #2931 ) ;
#13850 = VECTOR ( 'NONE', #12427, 1000.000000000000000 ) ;
#13851 = VERTEX_POINT ( 'NONE', #8098 ) ;
#13852 = CARTESIAN_POINT ( 'NONE',  ( 65.64431122251959039, 0.000000000000000000, -11.29787305743958115 ) ) ;
#13853 = AXIS2_PLACEMENT_3D ( 'NONE', #684, #14202, #16181 ) ;
#13854 = VECTOR ( 'NONE', #2325, 1000.000000000000000 ) ;
#13855 = CARTESIAN_POINT ( 'NONE',  ( 9.425811793576164277, 16.82642761605352888, 7.967843750810155612 ) ) ;
#13856 = CARTESIAN_POINT ( 'NONE',  ( 2.468147855947524505, 19.25811192615784151, 1.016953072036343997 ) ) ;
#13857 = CARTESIAN_POINT ( 'NONE',  ( 70.64340948846358970, 32.54502000000000095, -10.93409647675949969 ) ) ;
#13858 = CARTESIAN_POINT ( 'NONE',  ( 5.610206909946246157, 14.39083947916401662, -0.9654280252086245850 ) ) ;
#13859 = CIRCLE ( 'NONE', #7113, 0.5079999999999997851 ) ;
#13860 = DIRECTION ( 'NONE',  ( 0.08420877549337300871, 0.000000000000000000, 0.9964481331860212121 ) ) ;
#13861 = CARTESIAN_POINT ( 'NONE',  ( 6.780578452629304920, 10.88474977364208129, 3.138707800202942710 ) ) ;
#13862 = CARTESIAN_POINT ( 'NONE',  ( 5.103210221467147534, 12.69041179827479127, 6.197607713142090802 ) ) ;
#13863 = APPLICATION_CONTEXT ( 'automotive_design' ) ;
#13864 = EDGE_CURVE ( 'NONE', #15795, #17763, #6122, .T. ) ;
#13865 = FACE_OUTER_BOUND ( 'NONE', #1215, .T. ) ;
#13866 = CARTESIAN_POINT ( 'NONE',  ( 1.578497903329783236, 17.33698837102782520, 9.617339370494299544 ) ) ;
#13867 = CARTESIAN_POINT ( 'NONE',  ( 0.9078720132265757359, 19.93072420684222124, 8.031871908601623034 ) ) ;
#13868 = CIRCLE ( 'NONE', #4325, 22.02656249999999005 ) ;
#13869 = CARTESIAN_POINT ( 'NONE',  ( 37.13209340688868565, -6.356984999999999886, -3.529402718062123689 ) ) ;
#13870 = CARTESIAN_POINT ( 'NONE',  ( 11.07961582054159244, 20.23395749999999893, -3.332761710603877159 ) ) ;
#13871 = CARTESIAN_POINT ( 'NONE',  ( 42.94469661997857912, -1.983739999999999837, -18.48251861828712705 ) ) ;
#13872 = FACE_OUTER_BOUND ( 'NONE', #5493, .T. ) ;
#13873 = CARTESIAN_POINT ( 'NONE',  ( 17.67562427043129247, -8.149893664446995700, -15.71149448160998752 ) ) ;
#13874 = FACE_OUTER_BOUND ( 'NONE', #1187, .T. ) ;
#13875 = AXIS2_PLACEMENT_3D ( 'NONE', #6514, #11704, #10042 ) ;
#13876 = ADVANCED_FACE ( 'NONE', ( #4580, #13107, #4895 ), #18378, .F. ) ;
#13877 = FACE_OUTER_BOUND ( 'NONE', #11555, .T. ) ;
#13878 = VECTOR ( 'NONE', #7520, 1000.000000000000000 ) ;
#13879 = ADVANCED_FACE ( 'NONE', ( #8418 ), #10092, .T. ) ;
#13880 = CARTESIAN_POINT ( 'NONE',  ( 7.735533989518945219, 24.59767750000000319, -21.17236077523805449 ) ) ;
#13881 = CARTESIAN_POINT ( 'NONE',  ( 9.071911524784843195, 21.82902542499374476, 1.628992493446408396 ) ) ;
#13882 = DIRECTION ( 'NONE',  ( 0.5222415575336524229, 0.000000000000000000, 0.8527976052879281399 ) ) ;
#13883 = CARTESIAN_POINT ( 'NONE',  ( 11.31520137981316410, 12.97204149252575611, -2.348193457568243492 ) ) ;
#13884 = LINE ( 'NONE', #1908, #13055 ) ;
#13885 = CARTESIAN_POINT ( 'NONE',  ( 6.724285126367631094, 12.26967076330688222, 5.725847290954301450 ) ) ;
#13886 = VERTEX_POINT ( 'NONE', #15528 ) ;
#13887 = SHAPE_DEFINITION_REPRESENTATION ( #13969, #3526 ) ;
#13888 = CARTESIAN_POINT ( 'NONE',  ( 30.74535937054756829, -1.983739999999999393, -3.684081112461307317 ) ) ;
#13889 = VECTOR ( 'NONE', #13926, 1000.000000000000000 ) ;
#13890 = CARTESIAN_POINT ( 'NONE',  ( 4.730636513238291485, 20.15959900865225762, 1.386152104603439073 ) ) ;
#13891 = PLANE ( 'NONE',  #13244 ) ;
#13892 = AXIS2_PLACEMENT_3D ( 'NONE', #20458, #9987, #8748 ) ;
#13893 = ORIENTED_EDGE ( 'NONE', *, *, #15112, .T. ) ;
#13894 = COLOUR_RGB ( '', 0.31764706, 0.68627451, 0.89019608) ;
#13895 = CARTESIAN_POINT ( 'NONE',  ( 11.32746420189878656, 18.10709300986449222, -3.412108001743339170 ) ) ;
#13896 = CARTESIAN_POINT ( 'NONE',  ( 4.675198410806061133, 19.47349363154792812, 6.738369589952927896 ) ) ;
#13897 = EDGE_CURVE ( 'NONE', #7839, #17175, #3918, .T. ) ;
#13898 = CARTESIAN_POINT ( 'NONE',  ( 7.466363098872039750, 16.36411096495813311, -2.231798236382281697 ) ) ;
#13899 = CARTESIAN_POINT ( 'NONE',  ( 7.761792451437417029, 13.22675071421554094, 6.967738278329483670 ) ) ;
#13900 = EDGE_CURVE ( 'NONE', #9387, #9108, #13647, .T. ) ;
#13901 = CARTESIAN_POINT ( 'NONE',  ( 5.306437989180502690, 15.44500604033330404, -2.180778496895487528 ) ) ;
#13902 = ADVANCED_FACE ( 'NONE', ( #18923 ), #6770, .T. ) ;
#13903 = LINE ( 'NONE', #20600, #153 ) ;
#13904 = VECTOR ( 'NONE', #8590, 1000.000000000000000 ) ;
#13905 = CARTESIAN_POINT ( 'NONE',  ( 13.53491954000547537, 0.3256306608586702067, -16.21769529983032143 ) ) ;
#13906 = DIRECTION ( 'NONE',  ( 0.9579671649362033747, 0.000000000000000000, -0.2868778675745006779 ) ) ;
#13907 = VERTEX_POINT ( 'NONE', #3571 ) ;
#13908 = CARTESIAN_POINT ( 'NONE',  ( 8.179209644894292808, 10.68807868122940263, 1.726742278678839337 ) ) ;
#13909 = VERTEX_POINT ( 'NONE', #5437 ) ;
#13910 = CARTESIAN_POINT ( 'NONE',  ( 10.56155824565360923, 11.55374880816059324, 3.303473780892424827 ) ) ;
#13911 = CARTESIAN_POINT ( 'NONE',  ( 38.82016491058538321, 34.52875999999999124, -14.75770094105646812 ) ) ;
#13912 = CARTESIAN_POINT ( 'NONE',  ( 12.13621795668766445, -1.983739999999999393, 4.225309685850866082 ) ) ;
#13913 = AXIS2_PLACEMENT_3D ( 'NONE', #6654, #13414, #8410 ) ;
#13915 = DIRECTION ( 'NONE',  ( 0.000000000000000000, -1.000000000000000000, -0.000000000000000000 ) ) ;
#13914 = CARTESIAN_POINT ( 'NONE',  ( 3.080897780363576643, 18.24815116393151015, 8.946422692470362037 ) ) ;
#13916 = ORIENTED_EDGE ( 'NONE', *, *, #11997, .T. ) ;
#13917 =( NAMED_UNIT ( * ) SI_UNIT ( $, .STERADIAN. ) SOLID_ANGLE_UNIT ( ) );
#13918 = ORIENTED_EDGE ( 'NONE', *, *, #13709, .F. ) ;
#13919 = CARTESIAN_POINT ( 'NONE',  ( 0.03026019913916072612, 15.50729429995752007, 0.8891892028274968052 ) ) ;
#13920 = VECTOR ( 'NONE', #5489, 1000.000000000000114 ) ;
#13921 = DIRECTION ( 'NONE',  ( 0.000000000000000000, -1.000000000000000000, -0.000000000000000000 ) ) ;
#13922 = ORIENTED_EDGE ( 'NONE', *, *, #18198, .F. ) ;
#13923 = LINE ( 'NONE', #14353, #2926 ) ;
#13924 = EDGE_CURVE ( 'NONE', #3406, #6199, #17167, .T. ) ;
#13925 = AXIS2_PLACEMENT_3D ( 'NONE', #790, #14302, #4004 ) ;
#13926 = DIRECTION ( 'NONE',  ( 0.000000000000000000, 1.000000000000000000, 0.000000000000000000 ) ) ;
#13927 = DIRECTION ( 'NONE',  ( -0.7421532822901572013, 0.000000000000000000, 0.6702301885068637777 ) ) ;
#13928 = DIRECTION ( 'NONE',  ( 0.9237641507921645623, 0.000000000000000000, 0.3829618697876213673 ) ) ;
#13929 = DIRECTION ( 'NONE',  ( -0.6287118719681975554, 0.000000000000000000, -0.7776383362760898033 ) ) ;
#13930 = VERTEX_POINT ( 'NONE', #20456 ) ;
#13931 = LINE ( 'NONE', #3847, #1530 ) ;
#13932 = FACE_OUTER_BOUND ( 'NONE', #9367, .T. ) ;
#13934 = CARTESIAN_POINT ( 'NONE',  ( 17.80829803891473873, -6.635392327357950037, -14.48986153923296172 ) ) ;
#13933 = LINE ( 'NONE', #85, #14123 ) ;
#13935 = AXIS2_PLACEMENT_3D ( 'NONE', #16359, #21529, #9702 ) ;
#13936 = VERTEX_POINT ( 'NONE', #18592 ) ;
#13937 = VERTEX_POINT ( 'NONE', #248 ) ;
#13938 = CARTESIAN_POINT ( 'NONE',  ( 11.05478475839636232, 16.27078549497850091, -3.664008041822284678 ) ) ;
#13940 = CARTESIAN_POINT ( 'NONE',  ( 11.26949333533593922, -4.616615725918594038, -15.82154907933577448 ) ) ;
#13939 = CARTESIAN_POINT ( 'NONE',  ( 3.030261223045108476, 19.78000251358870187, 7.990636196055694640 ) ) ;
#13941 = ORIENTED_EDGE ( 'NONE', *, *, #14688, .T. ) ;
#13943 = CARTESIAN_POINT ( 'NONE',  ( 17.90945013363836580, -8.300072463023354885, -14.29531981980184163 ) ) ;
#13942 = CARTESIAN_POINT ( 'NONE',  ( 4.170163828269353168, 11.37233773221519151, 2.030869314271058101 ) ) ;
#13944 = ORIENTED_EDGE ( 'NONE', *, *, #9141, .T. ) ;
#13945 = VERTEX_POINT ( 'NONE', #18491 ) ;
#13946 = CARTESIAN_POINT ( 'NONE',  ( 7.601397047067438351, 17.55424594826779128, -1.993577623704449575 ) ) ;
#13947 = MANIFOLD_SOLID_BREP ( 'Stock-MAS-676-1', #3239 ) ;
#13948 = ORIENTED_EDGE ( 'NONE', *, *, #5626, .F. ) ;
#13949 = CIRCLE ( 'NONE', #12164, 0.5953125000000005773 ) ;
#13950 = ADVANCED_FACE ( 'NONE', ( #3682 ), #17275, .T. ) ;
#13951 = CARTESIAN_POINT ( 'NONE',  ( 8.309975510178299274, 0.1179876263055810032, 9.409168191377061063 ) ) ;
#13952 = DIRECTION ( 'NONE',  ( -0.8609107660235848503, 0.000000000000000000, 0.5087559856598096175 ) ) ;
#13953 = CARTESIAN_POINT ( 'NONE',  ( 66.03921914090641110, 32.54502000000000095, -10.93409647675949969 ) ) ;
#13954 = CARTESIAN_POINT ( 'NONE',  ( 2.706655912361267458, 20.34229411180381675, 7.226032060704281612 ) ) ;
#13955 = DIRECTION ( 'NONE',  ( 0.000000000000000000, 1.000000000000000000, 0.000000000000000000 ) ) ;
#13956 = VERTEX_POINT ( 'NONE', #8747 ) ;
#13957 = CARTESIAN_POINT ( 'NONE',  ( 0.3171430137197577270, 15.65082615746288219, 0.2565623787687694723 ) ) ;
#13958 = AXIS2_PLACEMENT_3D ( 'NONE', #18479, #21694, #21795 ) ;
#13959 = CARTESIAN_POINT ( 'NONE',  ( 61.60152099976809126, 0.000000000000000000, -12.48877542598203405 ) ) ;
#13960 = LINE ( 'NONE', #5190, #7123 ) ;
#13961 =( NAMED_UNIT ( * ) SI_UNIT ( $, .STERADIAN. ) SOLID_ANGLE_UNIT ( ) );
#13962 = ORIENTED_EDGE ( 'NONE', *, *, #9543, .F. ) ;
#13963 = ORIENTED_EDGE ( 'NONE', *, *, #18264, .T. ) ;
#13964 = CARTESIAN_POINT ( 'NONE',  ( 7.123635696461563249, 18.22263143684711650, -2.172865895562870353 ) ) ;
#13965 = FACE_OUTER_BOUND ( 'NONE', #10597, .T. ) ;
#13966 = CARTESIAN_POINT ( 'NONE',  ( 13.28239733708039338, 13.17358900937307098, 6.289479045720847594 ) ) ;
#13967 = ORIENTED_EDGE ( 'NONE', *, *, #4217, .T. ) ;
#13968 = CIRCLE ( 'NONE', #15384, 0.5953125000000004663 ) ;
#13969 = PRODUCT_DEFINITION_SHAPE ( 'NONE', 'NONE',  #11551 ) ;
#13970 = ORIENTED_EDGE ( 'NONE', *, *, #19779, .T. ) ;
#13971 = LINE ( 'NONE', #6969, #19054 ) ;
#13972 = CARTESIAN_POINT ( 'NONE',  ( 9.026437793025710477, 11.56923703291080230, 5.398293960222889432 ) ) ;
#13973 = CARTESIAN_POINT ( 'NONE',  ( 1.351254500901492683, 13.15556036664986195, 7.512915273831200835 ) ) ;
#13974 = LINE ( 'NONE', #10514, #6276 ) ;
#13975 = CARTESIAN_POINT ( 'NONE',  ( 5.961261165759633940, 18.61877392896656147, -0.8433191557062420518 ) ) ;
#13976 = CARTESIAN_POINT ( 'NONE',  ( 7.107506517079237973, 17.78663461815678204, 7.406428215689759398 ) ) ;
#13977 = CARTESIAN_POINT ( 'NONE',  ( 55.52866846859686234, -3.968114999999999615, -11.12083858657437752 ) ) ;
#13978 = EDGE_CURVE ( 'NONE', #20529, #4584, #1678, .T. ) ;
#13979 = CARTESIAN_POINT ( 'NONE',  ( 13.67197232725310130, 16.73453105516203721, 6.764297440454364541 ) ) ;
#13980 = ADVANCED_FACE ( 'NONE', ( #13757 ), #21, .T. ) ;
#13981 = AXIS2_PLACEMENT_3D ( 'NONE', #12941, #19650, #9806 ) ;
#13982 = LINE ( 'NONE', #5537, #2615 ) ;
#13983 = CARTESIAN_POINT ( 'NONE',  ( 2.795715374130701480, 20.92518826319738068, 1.845909576047056522 ) ) ;
#13984 = CARTESIAN_POINT ( 'NONE',  ( 1.503723558945946115, 17.75019041696929278, 9.406929423142640800 ) ) ;
#13985 = DIRECTION ( 'NONE',  ( 0.000000000000000000, 1.000000000000000000, 0.000000000000000000 ) ) ;
#13986 = CARTESIAN_POINT ( 'NONE',  ( 1.306606356420245030, 13.15608644122636228, 7.525809141478054798 ) ) ;
#13987 = CARTESIAN_POINT ( 'NONE',  ( 28.87608719841374949, -6.752907499999998286, -15.73691681567849976 ) ) ;
#13988 = CARTESIAN_POINT ( 'NONE',  ( 19.93283111454340784, 0.1696482471589960683, -14.27155714560671207 ) ) ;
#13989 = LINE ( 'NONE', #19365, #8147 ) ;
#13990 = DIRECTION ( 'NONE',  ( -0.6702301885068630005, 0.000000000000000000, -0.7421532822901579785 ) ) ;
#13991 = CARTESIAN_POINT ( 'NONE',  ( 8.858306312843332364, 21.71400761653233147, 1.040450809158882661 ) ) ;
#13992 = EDGE_LOOP ( 'NONE', ( #20217, #18012, #7405, #1485, #18209 ) ) ;
#13993 = DIRECTION ( 'NONE',  ( 0.2490110332224850509, 0.000000000000000000, -0.9685006480810792739 ) ) ;
#13994 = CARTESIAN_POINT ( 'NONE',  ( 11.17581378589971308, 16.27188659041726737, -3.588801592582428146 ) ) ;
#13995 = CARTESIAN_POINT ( 'NONE',  ( 11.63830738372303486, -3.658157632752987443, -15.74169750891422837 ) ) ;
#13996 = VERTEX_POINT ( 'NONE', #20347 ) ;
#13997 = EDGE_CURVE ( 'NONE', #2204, #6731, #12090, .T. ) ;
#13998 = CIRCLE ( 'NONE', #7610, 0.5079999999999984528 ) ;
#13999 = PRESENTATION_STYLE_ASSIGNMENT (( #2471 ) ) ;
#14000 = CARTESIAN_POINT ( 'NONE',  ( 4.141737580667239627, 18.68175291836243090, -0.04791304144243380830 ) ) ;
#14001 = DIRECTION ( 'NONE',  ( 0.000000000000000000, 1.000000000000000000, 0.000000000000000000 ) ) ;
#14002 = CARTESIAN_POINT ( 'NONE',  ( 10.67348499102866555, -4.915146421765576257, -16.12107055749564921 ) ) ;
#14003 = EDGE_LOOP ( 'NONE', ( #4804, #2852, #21128, #6254 ) ) ;
#14004 = CARTESIAN_POINT ( 'NONE',  ( 10.77600359882631764, 21.11368617580202312, 0.2706713370999587198 ) ) ;
#14005 = ADVANCED_FACE ( 'NONE', ( #13874 ), #19473, .T. ) ;
#14006 = CARTESIAN_POINT ( 'NONE',  ( 10.79498092501055950, 19.11273924176536099, 6.089322568971846650 ) ) ;
#14007 = CARTESIAN_POINT ( 'NONE',  ( 4.076791092353339252, 13.85370291750471772, -0.6031074348338666402 ) ) ;
#14008 = CARTESIAN_POINT ( 'NONE',  ( 12.45036876921160029, 10.42934933986260049, 2.737140771311291410 ) ) ;
#14009 = FACE_OUTER_BOUND ( 'NONE', #1626, .T. ) ;
#14010 = EDGE_CURVE ( 'NONE', #16794, #535, #14204, .T. ) ;
#14011 = DIRECTION ( 'NONE',  ( -0.9037041334408598692, -0.3596272420165190220, -0.2323512126103423059 ) ) ;
#14012 = ORIENTED_EDGE ( 'NONE', *, *, #5270, .F. ) ;
#14013 = CARTESIAN_POINT ( 'NONE',  ( 5.472929299800822101, 17.41108386104152572, -2.181338777335867452 ) ) ;
#14014 = DIRECTION ( 'NONE',  ( 0.000000000000000000, 1.000000000000000000, 0.000000000000000000 ) ) ;
#14015 = ORIENTED_EDGE ( 'NONE', *, *, #18691, .T. ) ;
#14016 = CARTESIAN_POINT ( 'NONE',  ( 9.581330595514776505, 12.45782188202256258, -1.022525368604570772 ) ) ;
#14017 = CARTESIAN_POINT ( 'NONE',  ( 53.11256268526609858, -5.166360000000005392, -16.69599035565043366 ) ) ;
#14018 = CARTESIAN_POINT ( 'NONE',  ( 4.936390548048069427, 34.12394749999999988, -19.84313358055101517 ) ) ;
#14020 = DIRECTION ( 'NONE',  ( 0.000000000000000000, -1.000000000000000000, 0.000000000000000000 ) ) ;
#14019 = CARTESIAN_POINT ( 'NONE',  ( 0.3421348966474949682, 11.72126458219154266, 4.984374349806848237 ) ) ;
#14021 = ORIENTED_EDGE ( 'NONE', *, *, #943, .T. ) ;
#14022 = CARTESIAN_POINT ( 'NONE',  ( 0.000000000000000000, 0.000000000000000000, 0.000000000000000000 ) ) ;
#14023 = EDGE_CURVE ( 'NONE', #7714, #1266, #20796, .T. ) ;
#14024 = EDGE_CURVE ( 'NONE', #10465, #4266, #14905, .T. ) ;
#14025 = VERTEX_POINT ( 'NONE', #2241 ) ;
#14026 = LINE ( 'NONE', #622, #4740 ) ;
#14027 = CARTESIAN_POINT ( 'NONE',  ( 20.37781590211399063, -3.328472077181156230, -15.39191602420292604 ) ) ;
#14028 = ORIENTED_EDGE ( 'NONE', *, *, #289, .T. ) ;
#14029 = DIRECTION ( 'NONE',  ( 0.000000000000000000, 1.000000000000000000, 0.000000000000000000 ) ) ;
#14030 = VECTOR ( 'NONE', #17813, 1000.000000000000114 ) ;
#14031 = CARTESIAN_POINT ( 'NONE',  ( 67.79270099634359781, 1.984375000000000000, -13.76558698117381851 ) ) ;
#14032 = CYLINDRICAL_SURFACE ( 'NONE', #19611, 0.7950199999999982836 ) ;
#14033 = DIRECTION ( 'NONE',  ( 0.000000000000000000, 1.000000000000000000, 0.000000000000000000 ) ) ;
#14034 = ORIENTED_EDGE ( 'NONE', *, *, #18725, .T. ) ;
#14035 = LINE ( 'NONE', #737, #4366 ) ;
#14036 = CARTESIAN_POINT ( 'NONE',  ( -5.132424380828760846, 25.39269750000000059, -7.958392962111297209 ) ) ;
#14037 = CARTESIAN_POINT ( 'NONE',  ( 21.05604118250877477, -1.172420585967219653, -15.20663495340546412 ) ) ;
#14039 = DIRECTION ( 'NONE',  ( -0.3140771401027085408, 0.9459569826691583971, -0.08075231887918271623 ) ) ;
#14038 = DIRECTION ( 'NONE',  ( 1.000000000000000000, 0.000000000000000000, 0.000000000000000000 ) ) ;
#14040 = ORIENTED_EDGE ( 'NONE', *, *, #16267, .T. ) ;
#14041 = VERTEX_POINT ( 'NONE', #5664 ) ;
#14042 = CARTESIAN_POINT ( 'NONE',  ( 6.135032277701231607, 11.87301092205614061, 1.607754465602344141 ) ) ;
#14044 = LINE ( 'NONE', #92, #14219 ) ;
#14043 = CARTESIAN_POINT ( 'NONE',  ( 4.186481793393173056, 11.26694048801452119, 1.988198107626873101 ) ) ;
#14045 = ORIENTED_EDGE ( 'NONE', *, *, #1811, .T. ) ;
#14047 = CARTESIAN_POINT ( 'NONE',  ( 10.64919035412082238, -4.868472515922345423, -15.50245527337344420 ) ) ;
#14046 = CARTESIAN_POINT ( 'NONE',  ( 4.268749360096856016, 11.23597362958910217, 2.456883663558785180 ) ) ;
#14048 = ORIENTED_EDGE ( 'NONE', *, *, #7025, .F. ) ;
#14049 = ADVANCED_FACE ( 'NONE', ( #12753 ), #5545, .F. ) ;
#14050 = AXIS2_PLACEMENT_3D ( 'NONE', #2289, #20626, #20738 ) ;
#14051 = ORIENTED_EDGE ( 'NONE', *, *, #17949, .T. ) ;
#14052 = CARTESIAN_POINT ( 'NONE',  ( 7.440635613041443719, 15.33804443884177893, -2.014925911322226426 ) ) ;
#14053 = CARTESIAN_POINT ( 'NONE',  ( 1.446457749880594168, 14.21890420874361638, 8.282590212535712482 ) ) ;
#14054 = ORIENTED_EDGE ( 'NONE', *, *, #1430, .F. ) ;
#14055 = DIRECTION ( 'NONE',  ( 0.000000000000000000, 1.000000000000000000, 0.000000000000000000 ) ) ;
#14056 = DIRECTION ( 'NONE',  ( 0.000000000000000000, 1.000000000000000000, 0.000000000000000000 ) ) ;
#14057 = DIRECTION ( 'NONE',  ( -0.1132953773954069460, 0.7241889112991807265, -0.6802312681817409556 ) ) ;
#14058 = CARTESIAN_POINT ( 'NONE',  ( 3.346841482731536921, 18.37601729971541786, 8.783708127353060391 ) ) ;
#14059 = CIRCLE ( 'NONE', #7693, 3.970020000000000326 ) ;
#14060 = EDGE_LOOP ( 'NONE', ( #8077, #18414, #19862, #21378 ) ) ;
#14061 = CARTESIAN_POINT ( 'NONE',  ( 3.984298728599178219, 15.55943979790526122, -0.8574646732594534138 ) ) ;
#14062 = CARTESIAN_POINT ( 'NONE',  ( -13.18827588824692754, 33.73373999999999739, -0.8886449702404607409 ) ) ;
#14063 = PLANE ( 'NONE',  #11684 ) ;
#14064 = LINE ( 'NONE', #447, #20178 ) ;
#14065 = ORIENTED_EDGE ( 'NONE', *, *, #19628, .T. ) ;
#14066 = ORIENTED_EDGE ( 'NONE', *, *, #19798, .F. ) ;
#14067 = CARTESIAN_POINT ( 'NONE',  ( 10.89219221246175273, 13.86399106732309328, 6.860601030035128112 ) ) ;
#14068 = LINE ( 'NONE', #3992, #13854 ) ;
#14069 = CARTESIAN_POINT ( 'NONE',  ( 11.51479575839695180, 11.09863041152549279, -1.273237637403870526 ) ) ;
#14070 = ORIENTED_EDGE ( 'NONE', *, *, #8842, .F. ) ;
#14071 = ORIENTED_EDGE ( 'NONE', *, *, #1415, .T. ) ;
#14072 = ADVANCED_FACE ( 'NONE', ( #15757 ), #17504, .T. ) ;
#14073 = LINE ( 'NONE', #20433, #2834 ) ;
#14074 = CARTESIAN_POINT ( 'NONE',  ( 7.336019681823533922, 17.38139003493714796, -2.801635840538051259 ) ) ;
#14075 = CARTESIAN_POINT ( 'NONE',  ( 2.476888523641526341, 19.25858774544496299, 1.013804407051679402 ) ) ;
#14076 = LINE ( 'NONE', #8963, #8400 ) ;
#14077 = CARTESIAN_POINT ( 'NONE',  ( 5.634997990689105229, 16.47394368154384381, -1.394772957107783151 ) ) ;
#14078 = CIRCLE ( 'NONE', #15140, 0.5080000000000023386 ) ;
#14079 = DIRECTION ( 'NONE',  ( -0.9173788132826627972, 0.000000000000000000, 0.3980152169705239440 ) ) ;
#14080 = CARTESIAN_POINT ( 'NONE',  ( 7.524408825705059201, 14.40990712224419745, -2.662676755242683324 ) ) ;
#14081 = CARTESIAN_POINT ( 'NONE',  ( 4.735151946278128854, 11.94990942969003633, 4.489362985911736104 ) ) ;
#14082 = CARTESIAN_POINT ( 'NONE',  ( -3.246390552019219999, 20.24316500000000119, 3.217431771123079987 ) ) ;
#14083 = CARTESIAN_POINT ( 'NONE',  ( 46.03750000000000142, 0.000000000000000000, -10.31874999999999964 ) ) ;
#14084 = CARTESIAN_POINT ( 'NONE',  ( 5.623058703637103584, 21.64257598718208442, 3.791041185262803204 ) ) ;
#14085 = DIRECTION ( 'NONE',  ( 0.000000000000000000, 1.000000000000000000, 0.000000000000000000 ) ) ;
#14086 = DIRECTION ( 'NONE',  ( 0.000000000000000000, 0.000000000000000000, 1.000000000000000000 ) ) ;
#14087 = CARTESIAN_POINT ( 'NONE',  ( 0.4365749149366086046, 12.38306287928572047, 3.436918907366315334 ) ) ;
#14088 = LINE ( 'NONE', #14310, #10964 ) ;
#14089 = LINE ( 'NONE', #16079, #18084 ) ;
#14090 = CARTESIAN_POINT ( 'NONE',  ( 17.29160225217250968, 2.068662977665156166, -15.07501658227938890 ) ) ;
#14091 = DIRECTION ( 'NONE',  ( 0.000000000000000000, 1.000000000000000000, 0.000000000000000000 ) ) ;
#14092 = CIRCLE ( 'NONE', #20760, 9.525000000000002132 ) ;
#14093 = DIRECTION ( 'NONE',  ( -0.2868778675745010664, 0.000000000000000000, -0.9579671649362032637 ) ) ;
#14094 = CARTESIAN_POINT ( 'NONE',  ( 10.67791946166693151, 10.86254514955002115, 3.740422676341600194 ) ) ;
#14095 = ORIENTED_EDGE ( 'NONE', *, *, #7217, .T. ) ;
#14096 = PRODUCT_DEFINITION_SHAPE ( 'NONE', 'NONE',  #17378 ) ;
#14097 = LINE ( 'NONE', #17404, #2171 ) ;
#14098 = ADVANCED_FACE ( 'NONE', ( #12422 ), #7653, .F. ) ;
#14099 = CARTESIAN_POINT ( 'NONE',  ( 12.27210225253973341, 11.22090649283593145, 1.901844011543860624 ) ) ;
#14100 = CARTESIAN_POINT ( 'NONE',  ( 6.053300999215300848, 11.21400605080730095, 1.403379422147501998 ) ) ;
#14101 = DIRECTION ( 'NONE',  ( -1.000000000000000000, 0.000000000000000000, 0.000000000000000000 ) ) ;
#14102 = ORIENTED_EDGE ( 'NONE', *, *, #19628, .F. ) ;
#14103 =( NAMED_UNIT ( * ) SI_UNIT ( $, .STERADIAN. ) SOLID_ANGLE_UNIT ( ) );
#14104 = CARTESIAN_POINT ( 'NONE',  ( 37.51913901087312553, 32.54502000000000095, -14.58057485080488114 ) ) ;
#14105 = FACE_BOUND ( 'NONE', #731, .T. ) ;
#14106 = AXIS2_PLACEMENT_3D ( 'NONE', #10371, #1853, #15372 ) ;
#14107 = CARTESIAN_POINT ( 'NONE',  ( 17.31620997348098356, 2.440699290912120123, -15.21585355587603416 ) ) ;
#14108 = ORIENTED_EDGE ( 'NONE', *, *, #12684, .T. ) ;
#14109 = CARTESIAN_POINT ( 'NONE',  ( 13.22401121011497871, 16.70014932840746980, 6.472590397630748171 ) ) ;
#14110 = CARTESIAN_POINT ( 'NONE',  ( 8.050360878220200078, 19.55923767994525875, -1.103070160109182796 ) ) ;
#14111 = PLANE ( 'NONE',  #17039 ) ;
#14112 = DIRECTION ( 'NONE',  ( 0.000000000000000000, 1.000000000000000000, 0.000000000000000000 ) ) ;
#14113 = ADVANCED_FACE ( 'NONE', ( #15648 ), #477, .F. ) ;
#14114 = VECTOR ( 'NONE', #3800, 1000.000000000000000 ) ;
#14115 = CARTESIAN_POINT ( 'NONE',  ( 19.65947855433865143, -1.905983633164971769, -14.27020732896038346 ) ) ;
#14116 = DIRECTION ( 'NONE',  ( 0.000000000000000000, -1.000000000000000000, 0.000000000000000000 ) ) ;
#14117 = VERTEX_POINT ( 'NONE', #10862 ) ;
#14118 = CARTESIAN_POINT ( 'NONE',  ( 13.28158503003489521, 12.74059347184058133, 6.139893691599064951 ) ) ;
#14119 = DIRECTION ( 'NONE',  ( 0.000000000000000000, 1.000000000000000000, 0.000000000000000000 ) ) ;
#14120 = ORIENTED_EDGE ( 'NONE', *, *, #18672, .T. ) ;
#14121 = EDGE_CURVE ( 'NONE', #21099, #13937, #13989, .T. ) ;
#14122 = CARTESIAN_POINT ( 'NONE',  ( 9.328167723008592205, 14.17953533357325213, -2.361609774951227703 ) ) ;
#14123 = VECTOR ( 'NONE', #6836, 1000.000000000000000 ) ;
#14124 = CARTESIAN_POINT ( 'NONE',  ( 42.66304184606194383, -9.531985000000000596, -19.22597499813143784 ) ) ;
#14125 = CARTESIAN_POINT ( 'NONE',  ( 8.505511374756364873, 39.28205249999999893, -20.97439202360551747 ) ) ;
#14126 = EDGE_CURVE ( 'NONE', #17778, #4193, #5693, .T. ) ;
#14127 = EDGE_CURVE ( 'NONE', #20855, #337, #1102, .T. ) ;
#14129 = FACE_OUTER_BOUND ( 'NONE', #17991, .T. ) ;
#14128 = CARTESIAN_POINT ( 'NONE',  ( 3.234135262388317056, 13.85370291750471772, -0.3507613039352304729 ) ) ;
#14130 = EDGE_LOOP ( 'NONE', ( #19932, #4093, #9062, #19405 ) ) ;
#14131 = CARTESIAN_POINT ( 'NONE',  ( 6.722042540637936270, 11.03467657806808155, 4.243594125539606132 ) ) ;
#14132 = DIRECTION ( 'NONE',  ( -0.000000000000000000, -1.000000000000000000, 0.000000000000000000 ) ) ;
#14133 = AXIS2_PLACEMENT_3D ( 'NONE', #5144, #8568, #15227 ) ;
#14134 = VERTEX_POINT ( 'NONE', #4120 ) ;
#14135 = CARTESIAN_POINT ( 'NONE',  ( 19.39017462591846197, 0.4351151282638252571, -14.99845457969487583 ) ) ;
#14136 = VECTOR ( 'NONE', #6641, 1000.000000000000000 ) ;
#14137 = CARTESIAN_POINT ( 'NONE',  ( 12.51650226353079276, -6.117377381860210406, -15.54956597296763832 ) ) ;
#14138 = VERTEX_POINT ( 'NONE', #15856 ) ;
#14139 = DIRECTION ( 'NONE',  ( 0.000000000000000000, 1.000000000000000000, 0.000000000000000000 ) ) ;
#14140 = DIRECTION ( 'NONE',  ( 0.000000000000000000, 1.000000000000000000, 0.000000000000000000 ) ) ;
#14141 = CARTESIAN_POINT ( 'NONE',  ( 3.805353748838121053, 34.52875999999999834, -22.18284873352824960 ) ) ;
#14142 = ADVANCED_FACE ( 'NONE', ( #686 ), #19031, .T. ) ;
#14143 = PRODUCT_DEFINITION_SHAPE ( 'NONE', 'NONE',  #19378 ) ;
#14144 = CARTESIAN_POINT ( 'NONE',  ( 43.29176983217143260, 37.11476346399999926, 5.154088326438659884 ) ) ;
#14145 = VERTEX_POINT ( 'NONE', #12538 ) ;
#14146 = CIRCLE ( 'NONE', #11637, 3.968750000000001776 ) ;
#14147 = CARTESIAN_POINT ( 'NONE',  ( -160.2647810241784896, 30.16440499999999858, 8.335010000000000474 ) ) ;
#14148 = FACE_OUTER_BOUND ( 'NONE', #19569, .T. ) ;
#14149 = CARTESIAN_POINT ( 'NONE',  ( 11.47063021243275394, -6.402320148554772494, -17.10925296469930146 ) ) ;
#14150 = LINE ( 'NONE', #7379, #5552 ) ;
#14151 = ORIENTED_EDGE ( 'NONE', *, *, #15694, .T. ) ;
#14152 = ORIENTED_EDGE ( 'NONE', *, *, #157, .T. ) ;
#14153 = EDGE_CURVE ( 'NONE', #8481, #14418, #6035, .T. ) ;
#14155 = DIRECTION ( 'NONE',  ( 0.000000000000000000, -1.000000000000000000, -0.000000000000000000 ) ) ;
#14154 = CARTESIAN_POINT ( 'NONE',  ( 3.571986513017807230, 13.65508413018860168, -0.8205120656026146930 ) ) ;
#14156 = ORIENTED_EDGE ( 'NONE', *, *, #16862, .F. ) ;
#14157 = CARTESIAN_POINT ( 'NONE',  ( 5.560588701018165381, 14.03900692732092637, 8.286612247724049141 ) ) ;
#14158 = EDGE_LOOP ( 'NONE', ( #12763, #7410 ) ) ;
#14159 = VECTOR ( 'NONE', #2219, 1000.000000000000000 ) ;
#14160 = VERTEX_POINT ( 'NONE', #19263 ) ;
#14161 = CARTESIAN_POINT ( 'NONE',  ( 1.307674456180993205, 13.22153521441935631, 7.464550839006347083 ) ) ;
#14162 = VERTEX_POINT ( 'NONE', #17608 ) ;
#14163 = TOROIDAL_SURFACE ( 'NONE', #19772, 4.961572499999999941, 0.3962400000000000366 ) ;
#14164 = VECTOR ( 'NONE', #14116, 1000.000000000000000 ) ;
#14165 = DIRECTION ( 'NONE',  ( 0.000000000000000000, 1.000000000000000000, 0.000000000000000000 ) ) ;
#14166 = EDGE_CURVE ( 'NONE', #15906, #8103, #16304, .T. ) ;
#14167 = CARTESIAN_POINT ( 'NONE',  ( 46.03750000000000142, -1.983739999999999837, -10.31874999999999964 ) ) ;
#14168 = CARTESIAN_POINT ( 'NONE',  ( 12.57635667311951622, -3.968114999999999615, 1.354834321244424267 ) ) ;
#14169 = CARTESIAN_POINT ( 'NONE',  ( 1.241553966568222478, 21.00182112902565024, 3.306851382610512147 ) ) ;
#14170 = EDGE_CURVE ( 'NONE', #18658, #3169, #12641, .T. ) ;
#14171 = CIRCLE ( 'NONE', #4618, 1.984374999999998890 ) ;
#14172 = EDGE_LOOP ( 'NONE', ( #3472, #10139, #4174, #16839 ) ) ;
#14173 = CARTESIAN_POINT ( 'NONE',  ( 5.279151643709653285, 18.80848272075206040, 7.411774736893618432 ) ) ;
#14174 = CARTESIAN_POINT ( 'NONE',  ( 11.83349417906578260, -4.444366718845225606, -15.99739072961142305 ) ) ;
#14175 = CARTESIAN_POINT ( 'NONE',  ( 13.17913432789424455, 22.09378701703648318, 2.003858574039297125 ) ) ;
#14176 = DIRECTION ( 'NONE',  ( -0.8609107660235850723, 0.000000000000000000, 0.5087559856598092844 ) ) ;
#14177 = ORIENTED_EDGE ( 'NONE', *, *, #11557, .F. ) ;
#14178 = EDGE_LOOP ( 'NONE', ( #4455, #14722, #17582, #18338 ) ) ;
#14179 = CARTESIAN_POINT ( 'NONE',  ( 8.053807618826375858, 20.99150983053873887, 0.1441728028981547893 ) ) ;
#14180 = VECTOR ( 'NONE', #6923, 1000.000000000000000 ) ;
#14182 = CARTESIAN_POINT ( 'NONE',  ( 23.95208767691813279, 8.724202693596797786, -0.5056039973118116038 ) ) ;
#14181 = DIRECTION ( 'NONE',  ( 0.9579671649362032637, 0.000000000000000000, -0.2868778675745010664 ) ) ;
#14183 = CARTESIAN_POINT ( 'NONE',  ( 13.32555521554802347, 13.59179201149856731, 6.524269766134250581 ) ) ;
#14184 = VERTEX_POINT ( 'NONE', #21454 ) ;
#14185 = VERTEX_POINT ( 'NONE', #13595 ) ;
#14186 = DIRECTION ( 'NONE',  ( 0.8334497143791951279, 0.000000000000000000, 0.5525953072558960066 ) ) ;
#14187 = CARTESIAN_POINT ( 'NONE',  ( 7.217504064768158756, 15.13630231636019907, -2.750538542655735164 ) ) ;
#14188 = CARTESIAN_POINT ( 'NONE',  ( 6.711813954139214111, 19.52167825130506174, 6.475648147207831329 ) ) ;
#14189 = CARTESIAN_POINT ( 'NONE',  ( -24.20935654380574320, 39.45064500000000152, -25.29247038871795894 ) ) ;
#14190 = CARTESIAN_POINT ( 'NONE',  ( 5.672450816875850066, 16.90457802579262392, -1.372803282523601842 ) ) ;
#14191 = AXIS2_PLACEMENT_3D ( 'NONE', #8782, #20724, #7022 ) ;
#14192 = DIRECTION ( 'NONE',  ( 0.05085730733808142834, 0.000000000000000000, -0.9987059298363657467 ) ) ;
#14193 = DIRECTION ( 'NONE',  ( 0.000000000000000000, 1.000000000000000000, 0.000000000000000000 ) ) ;
#14194 = CARTESIAN_POINT ( 'NONE',  ( 11.44906460655527347, 16.27109148020024776, -4.209446567205482381 ) ) ;
#14195 = DIRECTION ( 'NONE',  ( 0.7421532822901579785, 0.000000000000000000, -0.6702301885068630005 ) ) ;
#14196 = CARTESIAN_POINT ( 'NONE',  ( 1.449957865217590181, 12.54475284465800300, 8.036837038674857325 ) ) ;
#14197 = CARTESIAN_POINT ( 'NONE',  ( 1.954387715434429795, 23.41816500000000190, 6.745605000000000295 ) ) ;
#14198 = EDGE_CURVE ( 'NONE', #14184, #18623, #18547, .T. ) ;
#14199 = DIRECTION ( 'NONE',  ( 0.000000000000000000, 1.000000000000000000, 0.000000000000000000 ) ) ;
#14200 = CARTESIAN_POINT ( 'NONE',  ( 2.821159705543409668, 12.03350028468612010, 5.087159923345644152 ) ) ;
#14201 = CARTESIAN_POINT ( 'NONE',  ( 29.76562500000000000, 1.984375000000000000, -4.317999999999999616 ) ) ;
#14202 = DIRECTION ( 'NONE',  ( -0.000000000000000000, -1.000000000000000000, 0.000000000000000000 ) ) ;
#14203 = CARTESIAN_POINT ( 'NONE',  ( 17.39128954282556450, 2.036810952640657479, -15.04541658584163777 ) ) ;
#14204 = LINE ( 'NONE', #9307, #6405 ) ;
#14205 = CIRCLE ( 'NONE', #1124, 1.190625000000000711 ) ;
#14206 = AXIS2_PLACEMENT_3D ( 'NONE', #15834, #17481, #1988 ) ;
#14207 = LINE ( 'NONE', #20922, #12409 ) ;
#14208 = CARTESIAN_POINT ( 'NONE',  ( 11.23769815086176038, 12.55470729765644577, 6.205490070020298177 ) ) ;
#14209 = ORIENTED_EDGE ( 'NONE', *, *, #2487, .F. ) ;
#14210 = CARTESIAN_POINT ( 'NONE',  ( 11.56192577415882816, -3.968114999999999615, 4.677561850332325299 ) ) ;
#14211 = VECTOR ( 'NONE', #13620, 1000.000000000000114 ) ;
#14212 = CARTESIAN_POINT ( 'NONE',  ( 11.58533050013644861, 11.88887413582774499, -1.080035739352499746 ) ) ;
#14213 = CARTESIAN_POINT ( 'NONE',  ( 5.440803762682732803, 16.93165822604456494, -2.129577970569525913 ) ) ;
#14214 = CARTESIAN_POINT ( 'NONE',  ( -17.46249999999999858, -0.3962399999999990929, 0.000000000000000000 ) ) ;
#14215 = CARTESIAN_POINT ( 'NONE',  ( 3.362212792910313830, 14.97059756667285058, 8.341616412569205607 ) ) ;
#14216 = VERTEX_POINT ( 'NONE', #14747 ) ;
#14217 = DIRECTION ( 'NONE',  ( -0.2868778675745010664, 0.000000000000000000, -0.9579671649362032637 ) ) ;
#14218 = PLANE ( 'NONE',  #13603 ) ;
#14219 = VECTOR ( 'NONE', #14155, 1000.000000000000000 ) ;
#14220 = ORIENTED_EDGE ( 'NONE', *, *, #16672, .F. ) ;
#14221 = CARTESIAN_POINT ( 'NONE',  ( 12.51631392633175821, 11.22339177084746176, 2.531244740403540749 ) ) ;
#14222 = CARTESIAN_POINT ( 'NONE',  ( 10.14492818048215383, 20.26472116815758184, -1.210351513573973081 ) ) ;
#14223 = CARTESIAN_POINT ( 'NONE',  ( 2.768558239392996612, 11.29961739780916119, 3.368077172965935784 ) ) ;
#14224 = CARTESIAN_POINT ( 'NONE',  ( 65.90927232300019512, 30.56064500000000095, -13.30734117861468135 ) ) ;
#14225 = EDGE_CURVE ( 'NONE', #9387, #1535, #19684, .T. ) ;
#14226 = VECTOR ( 'NONE', #8051, 1000.000000000000000 ) ;
#14227 = AXIS2_PLACEMENT_3D ( 'NONE', #19332, #12278, #12174 ) ;
#14228 = DIRECTION ( 'NONE',  ( 0.1831666983862991482, 0.000000000000000000, -0.9830818687180954418 ) ) ;
#14229 = CARTESIAN_POINT ( 'NONE',  ( 3.780217353292837590, 21.35532275365758892, 4.459463005498162325 ) ) ;
#14230 = CARTESIAN_POINT ( 'NONE',  ( 12.54743718934339647, -0.7300314971274215470, -16.54148741527033906 ) ) ;
#14231 = CARTESIAN_POINT ( 'NONE',  ( 13.28268573882264469, 19.39178765922512326, -19.83174211820151100 ) ) ;
#14232 = VERTEX_POINT ( 'NONE', #21348 ) ;
#14233 = CARTESIAN_POINT ( 'NONE',  ( 9.847866323654898224, 10.74839508995118109, 0.1972236645847412484 ) ) ;
#14234 = CARTESIAN_POINT ( 'NONE',  ( 3.360635606688116894, -14.84248999999999974, -20.45316710734507026 ) ) ;
#14235 = CIRCLE ( 'NONE', #11398, 0.5953125000000005773 ) ;
#14236 = VERTEX_POINT ( 'NONE', #18159 ) ;
#14237 = CARTESIAN_POINT ( 'NONE',  ( 9.298361730296520022, 14.82474458426707287, -2.615784524909192221 ) ) ;
#14238 = DIRECTION ( 'NONE',  ( -1.000000000000000000, 0.000000000000000000, 0.000000000000000000 ) ) ;
#14239 = CARTESIAN_POINT ( 'NONE',  ( 0.9969110339907100160, 18.71640230995546617, 8.094414359749949384 ) ) ;
#14241 = CYLINDRICAL_SURFACE ( 'NONE', #14901, 3.175000000000000711 ) ;
#14240 = CARTESIAN_POINT ( 'NONE',  ( 1.573239863039354036, 18.09708922108623241, 0.02106776903118079761 ) ) ;
#14242 = ORIENTED_EDGE ( 'NONE', *, *, #20870, .F. ) ;
#14243 = DIRECTION ( 'NONE',  ( 0.000000000000000000, -1.000000000000000000, 0.000000000000000000 ) ) ;
#14244 = CARTESIAN_POINT ( 'NONE',  ( 11.11006317807338561, -14.84248999999999974, 0.5252656612939419212 ) ) ;
#14245 = VERTEX_POINT ( 'NONE', #21242 ) ;
#14246 = VECTOR ( 'NONE', #21047, 1000.000000000000000 ) ;
#14247 = CARTESIAN_POINT ( 'NONE',  ( 19.36302365051818342, 0.2638603526202955019, -15.04631431230876615 ) ) ;
#14248 = EDGE_CURVE ( 'NONE', #3318, #19591, #11818, .T. ) ;
#14249 = CARTESIAN_POINT ( 'NONE',  ( 14.86522180462012876, -7.415116976227209555, -15.24400705011625767 ) ) ;
#14250 = ORIENTED_EDGE ( 'NONE', *, *, #6255, .T. ) ;
#14251 = CYLINDRICAL_SURFACE ( 'NONE', #18106, 1.190625000000001155 ) ;
#14252 = EDGE_CURVE ( 'NONE', #20800, #11378, #16290, .T. ) ;
#14253 = EDGE_CURVE ( 'NONE', #723, #8326, #4668, .T. ) ;
#14254 = LINE ( 'NONE', #5375, #9258 ) ;
#14255 = FACE_BOUND ( 'NONE', #19294, .T. ) ;
#14256 = CIRCLE ( 'NONE', #7183, 0.3962400000000018130 ) ;
#14257 = ORIENTED_EDGE ( 'NONE', *, *, #10124, .F. ) ;
#14258 = CARTESIAN_POINT ( 'NONE',  ( 29.36874999999999858, 9.921875000000000000, 8.731249999999999289 ) ) ;
#14259 = DIRECTION ( 'NONE',  ( -0.9987059298363657467, 0.000000000000000000, -0.05085730733808409287 ) ) ;
#14260 = VERTEX_POINT ( 'NONE', #11292 ) ;
#14261 = ORIENTED_EDGE ( 'NONE', *, *, #15650, .F. ) ;
#14263 = DIRECTION ( 'NONE',  ( 0.000000000000000000, 1.000000000000000000, 0.000000000000000000 ) ) ;
#14262 = CARTESIAN_POINT ( 'NONE',  ( 0.3901958476314392743, 11.62494085263212185, 3.152395423529554819 ) ) ;
#14264 = ORIENTED_EDGE ( 'NONE', *, *, #14516, .T. ) ;
#14265 = CARTESIAN_POINT ( 'NONE',  ( 5.037610691315365763, 11.52515137269489287, 5.758083063193782714 ) ) ;
#14266 = AXIS2_PLACEMENT_3D ( 'NONE', #9296, #7422, #9181 ) ;
#14267 = EDGE_LOOP ( 'NONE', ( #2988, #17328, #17346, #19897, #8712, #21641, #14264, #15580, #4667, #21746, #2137, #16877 ) ) ;
#14268 = VERTEX_POINT ( 'NONE', #6835 ) ;
#14269 = ADVANCED_FACE ( 'NONE', ( #9738 ), #7759, .F. ) ;
#14270 = CARTESIAN_POINT ( 'NONE',  ( 1.463311253929418410, 14.47771670469544247, 8.418734608934853370 ) ) ;
#14271 = VECTOR ( 'NONE', #20787, 1000.000000000000000 ) ;
#14272 = ORIENTED_EDGE ( 'NONE', *, *, #21680, .T. ) ;
#14273 = CARTESIAN_POINT ( 'NONE',  ( 2.788510799092093428, 12.08762853899515655, 4.857404785327848806 ) ) ;
#14274 = EDGE_CURVE ( 'NONE', #15662, #14810, #15612, .T. ) ;
#14275 = DIRECTION ( 'NONE',  ( 0.9964481331860212121, 0.000000000000000000, -0.08420877549337300871 ) ) ;
#14276 = CIRCLE ( 'NONE', #14646, 0.3962399999999980382 ) ;
#14277 = CARTESIAN_POINT ( 'NONE',  ( -1.880134707694870011, 20.24316500000000119, 7.779750394130780400 ) ) ;
#14278 = PRODUCT ( 'Pivot Pin', 'Pivot Pin', '', ( #10437 ) ) ;
#14279 = DIRECTION ( 'NONE',  ( 0.000000000000000000, 1.000000000000000000, 0.000000000000000000 ) ) ;
#14280 = CARTESIAN_POINT ( 'NONE',  ( 3.373764802772109661, 18.23923658461143660, 8.840318433877319748 ) ) ;
#14281 = ORIENTED_EDGE ( 'NONE', *, *, #3296, .F. ) ;
#14282 = CARTESIAN_POINT ( 'NONE',  ( 1.184790726613003997, 11.72126458219154266, 4.732028218908065575 ) ) ;
#14283 = CARTESIAN_POINT ( 'NONE',  ( 53.10651001381376091, 37.69740999999999786, -16.70269254552787075 ) ) ;
#14284 = FACE_OUTER_BOUND ( 'NONE', #1516, .T. ) ;
#14285 = ORIENTED_EDGE ( 'NONE', *, *, #21010, .T. ) ;
#14286 = ORIENTED_EDGE ( 'NONE', *, *, #6404, .F. ) ;
#14287 = CARTESIAN_POINT ( 'NONE',  ( 13.92088304628949835, 21.18286304486736427, 4.294626054287162376 ) ) ;
#14289 = DIRECTION ( 'NONE',  ( 0.9685006480810790519, 0.000000000000000000, 0.2490110332224857170 ) ) ;
#14288 = DIRECTION ( 'NONE',  ( 0.000000000000000000, 1.000000000000000000, 0.000000000000000000 ) ) ;
#14290 = CARTESIAN_POINT ( 'NONE',  ( 12.49114903281414435, 10.57457003121523265, 2.794588968605982160 ) ) ;
#14291 = EDGE_LOOP ( 'NONE', ( #20111, #12691, #1335, #10738 ) ) ;
#14292 = ORIENTED_EDGE ( 'NONE', *, *, #19882, .F. ) ;
#14293 = CARTESIAN_POINT ( 'NONE',  ( 12.13621795668766445, 36.51313500000000545, 4.225309685850866082 ) ) ;
#14294 = CARTESIAN_POINT ( 'NONE',  ( 8.060400974142371666, 10.89137254501747165, 1.302109054530725452 ) ) ;
#14295 = CARTESIAN_POINT ( 'NONE',  ( 4.134645168753052324, 18.69448487464559250, -0.1575769768225616096 ) ) ;
#14296 = CARTESIAN_POINT ( 'NONE',  ( -24.21104940531825633, -6.903720000000000745, -25.29232732678598339 ) ) ;
#14297 = EDGE_CURVE ( 'NONE', #16776, #15970, #14526, .T. ) ;
#14298 = CARTESIAN_POINT ( 'NONE',  ( 6.980081620662553554, 20.74003334725626857, 1.714263682474118200 ) ) ;
#14299 = VECTOR ( 'NONE', #17418, 1000.000000000000000 ) ;
#14300 = EDGE_CURVE ( 'NONE', #2958, #21060, #1739, .T. ) ;
#14301 = EDGE_CURVE ( 'NONE', #10096, #6476, #7819, .T. ) ;
#14302 = DIRECTION ( 'NONE',  ( 0.000000000000000000, 1.000000000000000000, 0.000000000000000000 ) ) ;
#14303 = CARTESIAN_POINT ( 'NONE',  ( 7.941166293774544194, 20.10612899863186342, -1.699484797600306685 ) ) ;
#14304 = AXIS2_PLACEMENT_3D ( 'NONE', #11307, #9427, #3023 ) ;
#14305 = FACE_OUTER_BOUND ( 'NONE', #3486, .T. ) ;
#14306 = CARTESIAN_POINT ( 'NONE',  ( 7.257894689705208791, 18.51518438473548045, 8.066618968152379665 ) ) ;
#14307 = CARTESIAN_POINT ( 'NONE',  ( 0.4987414016220624857, 20.62897293350240346, 6.972998423300798443 ) ) ;
#14308 = CARTESIAN_POINT ( 'NONE',  ( 29.64606458365116737, -7.547927499999999235, -15.53894806404596096 ) ) ;
#14309 = CARTESIAN_POINT ( 'NONE',  ( -0.6625952780925900010, 20.05113242023052322, 3.974854857413083309 ) ) ;
#14310 = CARTESIAN_POINT ( 'NONE',  ( -16.73439918454169018, -4.609114529603660415, -25.92417111164088084 ) ) ;
#14311 = DIRECTION ( 'NONE',  ( -0.2490110332224889089, -7.284927983104707832E-16, 0.9685006480810781637 ) ) ;
#14312 = CARTESIAN_POINT ( 'NONE',  ( 11.30450557499492348, -0.5489953149440882640, -16.88206917429806353 ) ) ;
#14313 = ORIENTED_EDGE ( 'NONE', *, *, #19826, .T. ) ;
#14314 = DIRECTION ( 'NONE',  ( -0.08420877549337300871, 0.000000000000000000, -0.9964481331860212121 ) ) ;
#14315 = CARTESIAN_POINT ( 'NONE',  ( 10.20092691626072501, 10.57410012085601281, 1.745687182084074029 ) ) ;
#14316 = ORIENTED_EDGE ( 'NONE', *, *, #14670, .F. ) ;
#14317 = FACE_OUTER_BOUND ( 'NONE', #21430, .T. ) ;
#14318 = CARTESIAN_POINT ( 'NONE',  ( 12.01826200721117921, 20.34182557837260674, -1.780941468847173637 ) ) ;
#14319 = CARTESIAN_POINT ( 'NONE',  ( 6.055248116062193375, 11.21101810703654245, 1.411743302974689307 ) ) ;
#14320 = CARTESIAN_POINT ( 'NONE',  ( 65.90927232300019512, 32.54502000000000095, -12.91110117861467899 ) ) ;
#14321 = CARTESIAN_POINT ( 'NONE',  ( 1.812277707583389574, 16.41892220718292705, 0.009655869164628197443 ) ) ;
#14322 = VERTEX_POINT ( 'NONE', #6098 ) ;
#14323 = DIRECTION ( 'NONE',  ( 0.000000000000000000, 1.000000000000000000, 0.000000000000000000 ) ) ;
#14324 = EDGE_CURVE ( 'NONE', #14947, #21357, #15145, .T. ) ;
#14325 = DIRECTION ( 'NONE',  ( 0.9579671649362032637, 0.000000000000000000, -0.2868778675745010664 ) ) ;
#14326 = ORIENTED_EDGE ( 'NONE', *, *, #12226, .F. ) ;
#14327 = CARTESIAN_POINT ( 'NONE',  ( 9.021865827675320304, 12.18989644830414321, 5.065564172291198375 ) ) ;
#14328 = CARTESIAN_POINT ( 'NONE',  ( 4.895015545045986904, 18.85334257715032891, 7.259427143975731411 ) ) ;
#14329 = CARTESIAN_POINT ( 'NONE',  ( 6.431837864969753404, 20.04762713518370276, 0.1993235301662593661 ) ) ;
#14330 = DIRECTION ( 'NONE',  ( -0.1132953773954069598, 0.7241889112991808375, -0.6802312681817410667 ) ) ;
#14331 = CARTESIAN_POINT ( 'NONE',  ( 53.54703079237917507, -7.412034712371206702, -16.17856510773101775 ) ) ;
#14332 = CARTESIAN_POINT ( 'NONE',  ( 5.321178521759295066, 18.30337503607197647, 8.427072287543769136 ) ) ;
#14333 = CARTESIAN_POINT ( 'NONE',  ( -17.46249999999999858, -0.3962399999999990929, 0.000000000000000000 ) ) ;
#14334 = ORIENTED_EDGE ( 'NONE', *, *, #4617, .T. ) ;
#14335 = CARTESIAN_POINT ( 'NONE',  ( 12.85747229756767318, 22.28580575005450370, 0.3837689773447273134 ) ) ;
#14336 = CARTESIAN_POINT ( 'NONE',  ( 52.97981640314721119, 40.08215061204786878, -16.84218317533225928 ) ) ;
#14337 = AXIS2_PLACEMENT_3D ( 'NONE', #13987, #13645, #13534 ) ;
#14338 = ADVANCED_BREP_SHAPE_REPRESENTATION ( '', ( #6428, #2234 ), #10885 ) ;
#14339 = ORIENTED_EDGE ( 'NONE', *, *, #2788, .T. ) ;
#14340 = CARTESIAN_POINT ( 'NONE',  ( 9.849116944258051731, 19.41443847587203564, -1.859163645420073285 ) ) ;
#14341 = CARTESIAN_POINT ( 'NONE',  ( 53.09665848877359196, 37.69747050103866570, -16.71358996384494233 ) ) ;
#14342 = CYLINDRICAL_SURFACE ( 'NONE', #7867, 0.7950200000000003930 ) ;
#14344 = DIRECTION ( 'NONE',  ( 0.2490110332224855227, 0.000000000000000000, -0.9685006480810791629 ) ) ;
#14343 = CARTESIAN_POINT ( 'NONE',  ( 1.435485551437910345, 20.88642215721691997, 5.084564560294345448 ) ) ;
#14345 = ORIENTED_EDGE ( 'NONE', *, *, #3670, .T. ) ;
#14346 = PLANE ( 'NONE',  #4629 ) ;
#14347 = ADVANCED_FACE ( 'NONE', ( #21865 ), #2784, .F. ) ;
#14348 = CARTESIAN_POINT ( 'NONE',  ( 1.538505192098342578, 9.095123825415061702, 8.691315493779447010 ) ) ;
#14349 = ORIENTED_EDGE ( 'NONE', *, *, #6253, .F. ) ;
#14350 = LINE ( 'NONE', #20730, #128 ) ;
#14351 = CARTESIAN_POINT ( 'NONE',  ( 19.45436729525584951, -5.351618512891932689, -14.30490051005982011 ) ) ;
#14352 = ORIENTED_EDGE ( 'NONE', *, *, #19357, .T. ) ;
#14353 = CARTESIAN_POINT ( 'NONE',  ( 32.52436584422698473, -1.983739999999999837, 1.884807767196291284 ) ) ;
#14354 = EDGE_CURVE ( 'NONE', #9392, #13360, #21229, .T. ) ;
#14355 = CARTESIAN_POINT ( 'NONE',  ( 11.00471620700651698, 14.15586088870902515, -4.094554156936994538 ) ) ;
#14356 = DIRECTION ( 'NONE',  ( -0.9790635044817342925, 0.000000000000000000, 0.2035550397114870846 ) ) ;
#14357 = VERTEX_POINT ( 'NONE', #18043 ) ;
#14358 = DIRECTION ( 'NONE',  ( -0.2868778675745010664, 0.000000000000000000, -0.9579671649362032637 ) ) ;
#14360 = LINE ( 'NONE', #10811, #3448 ) ;
#14359 = CARTESIAN_POINT ( 'NONE',  ( 23.77193158452286781, 3.565842500000000914, -15.00033089984030887 ) ) ;
#14361 = ORIENTED_EDGE ( 'NONE', *, *, #674, .F. ) ;
#14362 = ORIENTED_EDGE ( 'NONE', *, *, #1587, .F. ) ;
#14363 = CARTESIAN_POINT ( 'NONE',  ( 10.47858167127056106, -3.825101884021728349, -15.95313145255061116 ) ) ;
#14365 = CARTESIAN_POINT ( 'NONE',  ( 22.02657784715807665, 36.51313500000000545, -12.98906981665815330 ) ) ;
#14364 = CARTESIAN_POINT ( 'NONE',  ( 0.06131086484389459967, 12.52652910124526109, 1.659618942007908604 ) ) ;
#14366 = VERTEX_POINT ( 'NONE', #14643 ) ;
#14367 = CARTESIAN_POINT ( 'NONE',  ( 3.782569706950912991, 18.34578091050401838, -1.064631198517248967 ) ) ;
#14368 = ORIENTED_EDGE ( 'NONE', *, *, #11855, .T. ) ;
#14369 = EDGE_CURVE ( 'NONE', #18428, #4430, #4300, .T. ) ;
#14370 = EDGE_LOOP ( 'NONE', ( #4288, #9314, #10923, #19659 ) ) ;
#14371 = EDGE_CURVE ( 'NONE', #19273, #5598, #1630, .T. ) ;
#14372 = ORIENTED_EDGE ( 'NONE', *, *, #10577, .T. ) ;
#14373 = CARTESIAN_POINT ( 'NONE',  ( 3.098003633530906686, 12.58238514230527194, 6.297671215640997744 ) ) ;
#14374 = DIRECTION ( 'NONE',  ( -0.7421532822901579785, 0.000000000000000000, 0.6702301885068630005 ) ) ;
#14375 = DIRECTION ( 'NONE',  ( -0.9964481331860213231, 0.000000000000000000, 0.08420877549337311974 ) ) ;
#14376 = FACE_OUTER_BOUND ( 'NONE', #10226, .T. ) ;
#14377 = FACE_OUTER_BOUND ( 'NONE', #911, .T. ) ;
#14378 = CARTESIAN_POINT ( 'NONE',  ( 2.429351595637148975, 11.35538272796713244, 3.277950258183725207 ) ) ;
#14379 = VERTEX_POINT ( 'NONE', #18645 ) ;
#14380 = LINE ( 'NONE', #21533, #5394 ) ;
#14381 = LINE ( 'NONE', #14489, #15978 ) ;
#14382 = CARTESIAN_POINT ( 'NONE',  ( -29.36874999999999858, 32.54502000000000095, -3.968750000000000000 ) ) ;
#14383 = DIRECTION ( 'NONE',  ( 0.000000000000000000, 1.000000000000000000, 0.000000000000000000 ) ) ;
#14384 = EDGE_CURVE ( 'NONE', #8281, #777, #9825, .T. ) ;
#14385 = DIRECTION ( 'NONE',  ( -0.7421532822901579785, 0.000000000000000000, 0.6702301885068630005 ) ) ;
#14386 = EDGE_LOOP ( 'NONE', ( #15837, #1183, #15702, #6617 ) ) ;
#14387 = ORIENTED_EDGE ( 'NONE', *, *, #8171, .T. ) ;
#14388 = CARTESIAN_POINT ( 'NONE',  ( 12.13064228076788176, 20.23326750546686270, 5.472641854910515136 ) ) ;
#14389 = AXIS2_PLACEMENT_3D ( 'NONE', #4583, #17965, #6232 ) ;
#14391 = DIRECTION ( 'NONE',  ( 0.9129422336036140395, 0.000000000000000000, -0.4080888115384250225 ) ) ;
#14390 = CARTESIAN_POINT ( 'NONE',  ( 37.51913901087312553, 0.000000000000000000, -14.58057485080488114 ) ) ;
#14392 = CARTESIAN_POINT ( 'NONE',  ( 11.45377137136283530, 11.24886065122903211, -1.534485868486173521 ) ) ;
#14393 = VERTEX_POINT ( 'NONE', #2179 ) ;
#14394 = ORIENTED_EDGE ( 'NONE', *, *, #15751, .T. ) ;
#14395 = DIRECTION ( 'NONE',  ( 0.000000000000000000, 1.000000000000000000, 0.000000000000000000 ) ) ;
#14396 = EDGE_CURVE ( 'NONE', #17848, #18972, #13699, .T. ) ;
#14397 = CARTESIAN_POINT ( 'NONE',  ( 7.227849133945657201, 15.88119260777969366, -2.864944999438480799 ) ) ;
#14398 = CARTESIAN_POINT ( 'NONE',  ( 5.282564265860938413, 17.31893540436420764, 8.015543990791440976 ) ) ;
#14399 = EDGE_CURVE ( 'NONE', #19126, #2537, #3629, .T. ) ;
#14400 = CARTESIAN_POINT ( 'NONE',  ( 8.519789844685428548, 19.76956797718314007, 5.764066944484178556 ) ) ;
#14401 = CARTESIAN_POINT ( 'NONE',  ( -17.46249999999999858, -1.587500000000002132, 0.000000000000000000 ) ) ;
#14402 = VECTOR ( 'NONE', #2991, 1000.000000000000000 ) ;
#14403 = CARTESIAN_POINT ( 'NONE',  ( 9.146683264432596161, 11.49625537507852080, 5.482365255748488764 ) ) ;
#14404 = LINE ( 'NONE', #18242, #135 ) ;
#14405 = DIRECTION ( 'NONE',  ( 0.2490110332224848289, 0.000000000000000000, -0.9685006480810792739 ) ) ;
#14406 = CARTESIAN_POINT ( 'NONE',  ( 0.3457492210648637210, 11.62559268301756177, 3.165962217078898799 ) ) ;
#14407 = CARTESIAN_POINT ( 'NONE',  ( 1.703304774440397296, 15.10408740295005714, 9.458727078297481938 ) ) ;
#14408 = CYLINDRICAL_SURFACE ( 'NONE', #19527, 0.3962400000000000366 ) ;
#14409 = CARTESIAN_POINT ( 'NONE',  ( 5.951959548518082954, 12.27588422369934129, 0.9763157611141449754 ) ) ;
#14410 = CARTESIAN_POINT ( 'NONE',  ( 53.10651001381376091, 40.07865999999999929, -16.70269254552787075 ) ) ;
#14411 = CYLINDRICAL_SURFACE ( 'NONE', #20511, 0.7950200000000005041 ) ;
#14412 = CARTESIAN_POINT ( 'NONE',  ( 14.35329266030264961, 2.065734012470558767, -15.94383203165788210 ) ) ;
#14413 = EDGE_CURVE ( 'NONE', #6050, #138, #12250, .T. ) ;
#14414 = ORIENTED_EDGE ( 'NONE', *, *, #12739, .F. ) ;
#14415 = DIRECTION ( 'NONE',  ( -0.9987059298363656357, 0.000000000000000000, -0.05085730733808393328 ) ) ;
#14416 = EDGE_CURVE ( 'NONE', #16799, #21613, #8822, .T. ) ;
#14417 = CARTESIAN_POINT ( 'NONE',  ( 11.14903082554621605, 12.11221548192478004, 5.790615822781773225 ) ) ;
#14418 = VERTEX_POINT ( 'NONE', #527 ) ;
#14419 = CARTESIAN_POINT ( 'NONE',  ( 23.20826401227170166, 0.8126278217654899771, 10.33343709694782042 ) ) ;
#14420 = CARTESIAN_POINT ( 'NONE',  ( 12.08799520445995945, 20.48566632575741764, -1.599630408105054746 ) ) ;
#14421 = VECTOR ( 'NONE', #11837, 1000.000000000000227 ) ;
#14422 = CARTESIAN_POINT ( 'NONE',  ( 5.856409722658628247, 11.60590070312898092, 0.5491629594515322621 ) ) ;
#14423 = FACE_BOUND ( 'NONE', #5471, .T. ) ;
#14424 = ORIENTED_EDGE ( 'NONE', *, *, #11024, .T. ) ;
#14425 = FILL_AREA_STYLE ('',( #9641 ) ) ;
#14426 = CARTESIAN_POINT ( 'NONE',  ( 6.000401609189997210, 20.54164716138263813, 4.721118242335392345 ) ) ;
#14427 = DIRECTION ( 'NONE',  ( -0.7776383362760928009, 0.000000000000000000, 0.6287118719681937806 ) ) ;
#14428 = VERTEX_POINT ( 'NONE', #13810 ) ;
#14429 = CARTESIAN_POINT ( 'NONE',  ( 9.844264539218293919, 12.30663295771102383, -1.228584621700786306 ) ) ;
#14430 = CARTESIAN_POINT ( 'NONE',  ( 6.971783283983191026, 20.81512969834162163, 1.607819997509327692 ) ) ;
#14431 = CARTESIAN_POINT ( 'NONE',  ( 3.283575605484034821, 19.71984925633132235, 7.849616204200203562 ) ) ;
#14432 = LINE ( 'NONE', #18176, #9286 ) ;
#14433 = CARTESIAN_POINT ( 'NONE',  ( 16.85197508397059707, 19.43957250000000059, -16.77951971243562923 ) ) ;
#14434 = PLANE ( 'NONE',  #11494 ) ;
#14435 = EDGE_CURVE ( 'NONE', #10320, #16032, #15803, .T. ) ;
#14436 = ADVANCED_FACE ( 'NONE', ( #17218 ), #17977, .T. ) ;
#14437 = CARTESIAN_POINT ( 'NONE',  ( 32.52436584422698473, -1.983739999999999837, 1.884807767196291284 ) ) ;
#14438 = ORIENTED_EDGE ( 'NONE', *, *, #12212, .F. ) ;
#14439 =( GEOMETRIC_REPRESENTATION_CONTEXT ( 3 ) GLOBAL_UNCERTAINTY_ASSIGNED_CONTEXT ( ( #18729 ) ) GLOBAL_UNIT_ASSIGNED_CONTEXT ( ( #8229, #1267, #15105 ) ) REPRESENTATION_CONTEXT ( 'NONE', 'WORKASPACE' ) );
#14440 = CARTESIAN_POINT ( 'NONE',  ( 29.36874999999999858, 22.62187499999999929, 8.731249999999999289 ) ) ;
#14441 = ORIENTED_EDGE ( 'NONE', *, *, #9943, .F. ) ;
#14442 = CARTESIAN_POINT ( 'NONE',  ( 11.30859256852448347, 21.24860540534560016, 1.983546970420978939 ) ) ;
#14443 = CARTESIAN_POINT ( 'NONE',  ( 53.09009400389079758, 37.69765126434668190, -16.72082518125775863 ) ) ;
#14444 = CARTESIAN_POINT ( 'NONE',  ( 0.08608646803520518531, 20.17500070246044075, 5.848371221736313075 ) ) ;
#14445 = CARTESIAN_POINT ( 'NONE',  ( 13.92886986911328506, 2.297057816795145424, -15.92078612283740569 ) ) ;
#14447 = DIRECTION ( 'NONE',  ( 0.7421532822901579785, 0.000000000000000000, -0.6702301885068628895 ) ) ;
#14446 = CARTESIAN_POINT ( 'NONE',  ( -0.7373233266190051260, 20.71056957386564079, 4.930574937443840788 ) ) ;
#14448 = ORIENTED_EDGE ( 'NONE', *, *, #15336, .F. ) ;
#14449 = FACE_OUTER_BOUND ( 'NONE', #8573, .T. ) ;
#14450 = DIRECTION ( 'NONE',  ( -0.9564948366894091558, 0.05542109139015083397, 0.2864369564417712510 ) ) ;
#14451 = AXIS2_PLACEMENT_3D ( 'NONE', #16396, #16717, #6309 ) ;
#14452 = ORIENTED_EDGE ( 'NONE', *, *, #26, .T. ) ;
#14453 = FACE_OUTER_BOUND ( 'NONE', #19120, .T. ) ;
#14454 = CARTESIAN_POINT ( 'NONE',  ( 0.5053304282907709055, 18.78275443002634759, 1.545950046922383025 ) ) ;
#14455 = CARTESIAN_POINT ( 'NONE',  ( 19.61166229506757475, -5.924300855026435109, -15.80696905612679792 ) ) ;
#14456 = ORIENTED_EDGE ( 'NONE', *, *, #17647, .T. ) ;
#14457 = CARTESIAN_POINT ( 'NONE',  ( 12.86047607407836324, 18.46447794879854243, 6.079284020093307817 ) ) ;
#14458 = CARTESIAN_POINT ( 'NONE',  ( 2.418392266879479724, 19.05216738376148911, 0.9656792871569455095 ) ) ;
#14459 = CARTESIAN_POINT ( 'NONE',  ( 11.21401574228518427, 12.31537751810604320, -3.001107651909319607 ) ) ;
#14460 = EDGE_CURVE ( 'NONE', #19233, #17007, #144, .T. ) ;
#14461 = FACE_BOUND ( 'NONE', #10031, .T. ) ;
#14462 = VECTOR ( 'NONE', #195, 1000.000000000000000 ) ;
#14463 = VERTEX_POINT ( 'NONE', #20582 ) ;
#14464 = FACE_OUTER_BOUND ( 'NONE', #13708, .T. ) ;
#14465 = LINE ( 'NONE', #12363, #4161 ) ;
#14466 = ORIENTED_EDGE ( 'NONE', *, *, #6027, .F. ) ;
#14467 = ORIENTED_EDGE ( 'NONE', *, *, #9373, .F. ) ;
#14468 = CYLINDRICAL_SURFACE ( 'NONE', #5619, 0.3962399999999998146 ) ;
#14470 = DIRECTION ( 'NONE',  ( -0.2035550397114870846, 0.000000000000000000, -0.9790635044817342925 ) ) ;
#14469 = CARTESIAN_POINT ( 'NONE',  ( 3.929373626785105600, 19.12659651351990320, -0.8107010527169089542 ) ) ;
#14471 = ORIENTED_EDGE ( 'NONE', *, *, #3722, .F. ) ;
#14472 = EDGE_CURVE ( 'NONE', #21393, #11391, #589, .T. ) ;
#14473 = CARTESIAN_POINT ( 'NONE',  ( 3.950319039265778986, 19.11221838521101546, -0.6870736532921090101 ) ) ;
#14474 = VECTOR ( 'NONE', #5990, 1000.000000000000000 ) ;
#14475 = B_SPLINE_CURVE_WITH_KNOTS ( 'NONE', 3,
 ( #8670, #8447, #3485, #10221, #10553, #7012, #384, #2029, #12223, #1818 ),
 .UNSPECIFIED., .F., .F.,
 ( 4, 2, 2, 2, 4 ),
 ( 0.000000000000000000, 0.2500000000000017764, 0.5000000000000011102, 0.7500000000000005551, 1.000000000000000000 ),
 .UNSPECIFIED. ) ;
#14476 = VERTEX_POINT ( 'NONE', #16947 ) ;
#14477 = ORIENTED_EDGE ( 'NONE', *, *, #12105, .F. ) ;
#14478 = CARTESIAN_POINT ( 'NONE',  ( 0.8869166634311153041, 12.25464994366603122, 5.429115086724404016 ) ) ;
#14479 = ORIENTED_EDGE ( 'NONE', *, *, #9889, .T. ) ;
#14480 = CIRCLE ( 'NONE', #343, 0.7950199999999988387 ) ;
#14481 = FACE_OUTER_BOUND ( 'NONE', #18252, .T. ) ;
#14482 = DIRECTION ( 'NONE',  ( -0.2868778675745011220, 0.000000000000000000, -0.9579671649362033747 ) ) ;
#14483 = FACE_OUTER_BOUND ( 'NONE', #10983, .T. ) ;
#14484 = CARTESIAN_POINT ( 'NONE',  ( 19.99312429566830218, -1.983739999999999393, -11.46559883803463720 ) ) ;
#14485 = CARTESIAN_POINT ( 'NONE',  ( 2.832812540163568649, 11.30610737436141200, 5.018348456016711090 ) ) ;
#14486 = EDGE_CURVE ( 'NONE', #11160, #16300, #17062, .T. ) ;
#14487 = VERTEX_POINT ( 'NONE', #2128 ) ;
#14488 = FACE_BOUND ( 'NONE', #20647, .T. ) ;
#14489 = CARTESIAN_POINT ( 'NONE',  ( 29.15193331460030279, 39.28205249999999893, -13.61707959051006966 ) ) ;
#14490 = CARTESIAN_POINT ( 'NONE',  ( 13.00571045122730851, 21.87905377962147213, 2.024278336491688535 ) ) ;
#14491 = CARTESIAN_POINT ( 'NONE',  ( 3.360635606688116894, 34.52875999999999834, -20.45316710734507026 ) ) ;
#14492 = ORIENTED_EDGE ( 'NONE', *, *, #11413, .F. ) ;
#14493 = VERTEX_POINT ( 'NONE', #18930 ) ;
#14494 = CARTESIAN_POINT ( 'NONE',  ( 7.707318447941210238, 19.61749303057682070, -1.067354726136881427 ) ) ;
#14495 = VECTOR ( 'NONE', #15429, 1000.000000000000114 ) ;
#14497 = FACE_OUTER_BOUND ( 'NONE', #13307, .T. ) ;
#14496 = FACE_BOUND ( 'NONE', #9574, .T. ) ;
#14498 = CARTESIAN_POINT ( 'NONE',  ( 11.08491485109335351, 17.82867876252078432, -4.185153311738524451 ) ) ;
#14499 = ORIENTED_EDGE ( 'NONE', *, *, #19795, .F. ) ;
#14500 = EDGE_LOOP ( 'NONE', ( #9243, #4715, #16293, #3090 ) ) ;
#14501 = DIRECTION ( 'NONE',  ( -1.000000000000000000, 0.000000000000000000, 0.000000000000000000 ) ) ;
#14502 = CARTESIAN_POINT ( 'NONE',  ( 7.261604238741163897, 13.94690558326506746, -2.355022785685753739 ) ) ;
#14503 = LINE ( 'NONE', #6079, #994 ) ;
#14504 = AXIS2_PLACEMENT_3D ( 'NONE', #13871, #2348, #17501 ) ;
#14505 = AXIS2_PLACEMENT_3D ( 'NONE', #16339, #4828, #15119 ) ;
#14506 = CARTESIAN_POINT ( 'NONE',  ( 6.388697458777018667, 19.89557336115347397, 0.1802627198813876175 ) ) ;
#14507 = CYLINDRICAL_SURFACE ( 'NONE', #3658, 22.02656249999999361 ) ;
#14508 = EDGE_CURVE ( 'NONE', #10511, #513, #8541, .T. ) ;
#14509 = VECTOR ( 'NONE', #11747, 1000.000000000000000 ) ;
#14510 = CARTESIAN_POINT ( 'NONE',  ( 5.544310973761614747, 17.41197255053186055, -2.207093946540664042 ) ) ;
#14511 = DIRECTION ( 'NONE',  ( 0.7421532822901579785, 0.000000000000000000, -0.6702301885068630005 ) ) ;
#14512 = DIRECTION ( 'NONE',  ( 0.000000000000000000, -1.000000000000000000, 0.000000000000000000 ) ) ;
#14513 = PLANE ( 'NONE',  #1916 ) ;
#14514 = CARTESIAN_POINT ( 'NONE',  ( 0.9415645308267408531, 11.48439724119077177, 5.634514928165719638 ) ) ;
#14515 = EDGE_CURVE ( 'NONE', #17451, #8841, #10907, .T. ) ;
#14516 = EDGE_CURVE ( 'NONE', #13956, #8026, #18709, .T. ) ;
#14517 = EDGE_CURVE ( 'NONE', #4173, #16563, #10433, .T. ) ;
#14518 = DIRECTION ( 'NONE',  ( 0.000000000000000000, 0.000000000000000000, -1.000000000000000000 ) ) ;
#14519 = CIRCLE ( 'NONE', #9555, 15.47812499999999680 ) ;
#14520 = CARTESIAN_POINT ( 'NONE',  ( 5.034481523711040296, 20.64273285859446361, 2.220149373443666807 ) ) ;
#14521 = CARTESIAN_POINT ( 'NONE',  ( 1.786968685778054455, 23.59452865405863875, 10.71398755195300900 ) ) ;
#14522 = CARTESIAN_POINT ( 'NONE',  ( 53.14266576735293768, -5.167590446840315543, -16.66242751532468702 ) ) ;
#14523 = CARTESIAN_POINT ( 'NONE',  ( 12.07693058128559649, -6.954572128932724695, -15.70789055935204281 ) ) ;
#14524 = VECTOR ( 'NONE', #1036, 1000.000000000000000 ) ;
#14525 = VERTEX_POINT ( 'NONE', #15322 ) ;
#14526 = LINE ( 'NONE', #19588, #17366 ) ;
#14527 = CARTESIAN_POINT ( 'NONE',  ( 10.79394434136722225, 11.05572186037332294, 4.232501299144526996 ) ) ;
#14528 = ORIENTED_EDGE ( 'NONE', *, *, #16291, .F. ) ;
#14529 = CIRCLE ( 'NONE', #8193, 1.984374999999998890 ) ;
#14530 = CARTESIAN_POINT ( 'NONE',  ( 19.64159472326995015, 0.5582924111307500104, 10.11216594088294052 ) ) ;
#14531 = CIRCLE ( 'NONE', #19777, 0.5079999999999985638 ) ;
#14532 = CARTESIAN_POINT ( 'NONE',  ( 5.627668837156483583, 18.34364325301588394, -1.803485302817334546 ) ) ;
#14533 = CARTESIAN_POINT ( 'NONE',  ( -29.36874999999999858, 0.000000000000000000, 10.71562499999999929 ) ) ;
#14534 = CARTESIAN_POINT ( 'NONE',  ( 6.586789902921174722, 11.71523883824356282, 4.117049529868094027 ) ) ;
#14535 = VECTOR ( 'NONE', #21515, 1000.000000000000114 ) ;
#14536 = ORIENTED_EDGE ( 'NONE', *, *, #21146, .T. ) ;
#14537 = LINE ( 'NONE', #18056, #5444 ) ;
#14538 = EDGE_CURVE ( 'NONE', #3944, #2217, #364, .T. ) ;
#14539 = CARTESIAN_POINT ( 'NONE',  ( 11.69938498582200914, 11.70279650494946289, -0.9857855139570842473 ) ) ;
#14540 = AXIS2_PLACEMENT_3D ( 'NONE', #14652, #1135, #16197 ) ;
#14541 = CARTESIAN_POINT ( 'NONE',  ( -1.345424459097947834, 20.24316500000000119, 2.648158502653860324 ) ) ;
#14542 = AXIS2_PLACEMENT_3D ( 'NONE', #3162, #4726, #19733 ) ;
#14543 = EDGE_CURVE ( 'NONE', #6593, #19545, #13884, .T. ) ;
#14544 = CIRCLE ( 'NONE', #1455, 0.3962399999999998146 ) ;
#14545 = DIRECTION ( 'NONE',  ( -0.2868778675745006224, -1.090993607693396258E-14, -0.9579671649362034858 ) ) ;
#14546 = DIRECTION ( 'NONE',  ( -0.9685006480810791629, 0.000000000000000000, -0.2490110332224850231 ) ) ;
#14547 = CARTESIAN_POINT ( 'NONE',  ( 20.78426922154476131, -5.262943049308428378, -15.07321085010084438 ) ) ;
#14548 = FACE_OUTER_BOUND ( 'NONE', #11919, .T. ) ;
#14549 = AXIS2_PLACEMENT_3D ( 'NONE', #12276, #20768, #9156 ) ;
#14550 = ORIENTED_EDGE ( 'NONE', *, *, #8739, .F. ) ;
#14551 = CYLINDRICAL_SURFACE ( 'NONE', #16703, 1.191259999999998209 ) ;
#14552 = AXIS2_PLACEMENT_3D ( 'NONE', #9190, #14314, #5879 ) ;
#14553 = DIRECTION ( 'NONE',  ( 0.000000000000000000, -1.000000000000000000, -0.000000000000000000 ) ) ;
#14554 = ORIENTED_EDGE ( 'NONE', *, *, #12357, .F. ) ;
#14555 = CARTESIAN_POINT ( 'NONE',  ( 12.23193311121828586, 20.35868270965967852, 4.448204119538093693 ) ) ;
#14556 = CARTESIAN_POINT ( 'NONE',  ( 1.459005598626311073, 16.01352310531106937, 8.842019805628964946 ) ) ;
#14557 = CARTESIAN_POINT ( 'NONE',  ( 19.70749945469935227, -6.234009617392132441, -14.61948376456804688 ) ) ;
#14559 = DIRECTION ( 'NONE',  ( 0.2868778675745010664, 0.000000000000000000, 0.9579671649362032637 ) ) ;
#14558 = CARTESIAN_POINT ( 'NONE',  ( -1.111594454113435715, 19.92362218466222146, 3.626275517597432607 ) ) ;
#14560 = EDGE_LOOP ( 'NONE', ( #16699, #9136, #2664, #15729 ) ) ;
#14561 = SHAPE_REPRESENTATION_RELATIONSHIP ( 'NONE' , 'NONE' ,  #17083, #13006 ) ;
#14562 = PLANE ( 'NONE',  #9919 ) ;
#14563 = CIRCLE ( 'NONE', #20868, 0.7950200000000000600 ) ;
#14564 = DIRECTION ( 'NONE',  ( 0.9636276526537417286, 0.000000000000000000, -0.2672484743474500268 ) ) ;
#14565 = AXIS2_PLACEMENT_3D ( 'NONE', #11289, #13191, #9833 ) ;
#14566 = VECTOR ( 'NONE', #1212, 1000.000000000000000 ) ;
#14567 = ORIENTED_EDGE ( 'NONE', *, *, #12188, .T. ) ;
#14568 = LINE ( 'NONE', #9776, #8279 ) ;
#14569 = EDGE_CURVE ( 'NONE', #12952, #18076, #12733, .T. ) ;
#14570 = EDGE_CURVE ( 'NONE', #12574, #14357, #15655, .T. ) ;
#14571 = CIRCLE ( 'NONE', #5008, 25.00312500000000426 ) ;
#14572 = EDGE_CURVE ( 'NONE', #17145, #6991, #6993, .T. ) ;
#14573 = CARTESIAN_POINT ( 'NONE',  ( 20.03605712096321412, -6.234006942471316925, -15.89736554983887906 ) ) ;
#14574 = ORIENTED_EDGE ( 'NONE', *, *, #12161, .F. ) ;
#14575 = AXIS2_PLACEMENT_3D ( 'NONE', #8076, #20106, #11942 ) ;
#14576 = CARTESIAN_POINT ( 'NONE',  ( 11.18302750797556655, 14.04470801367943267, 6.395837339788904785 ) ) ;
#14577 = CARTESIAN_POINT ( 'NONE',  ( 2.716457121344570069, 19.77266525423434729, 1.688395397584657953 ) ) ;
#14578 = CARTESIAN_POINT ( 'NONE',  ( 8.772911046456378870, 20.20056482616064031, 6.600680312436005615 ) ) ;
#14579 = APPLICATION_CONTEXT ( 'automotive_design' ) ;
#14580 = VECTOR ( 'NONE', #4082, 1000.000000000000000 ) ;
#14581 = CARTESIAN_POINT ( 'NONE',  ( 20.08848443642310144, -3.313481494631655089, -15.32311112960731414 ) ) ;
#14582 = DIRECTION ( 'NONE',  ( 0.000000000000000000, 1.000000000000000000, 0.000000000000000000 ) ) ;
#14583 = AXIS2_PLACEMENT_3D ( 'NONE', #9925, #2985, #14611 ) ;
#14584 = ORIENTED_EDGE ( 'NONE', *, *, #2598, .F. ) ;
#14585 = DIRECTION ( 'NONE',  ( 0.7421532822901569793, 0.000000000000000000, -0.6702301885068642218 ) ) ;
#14586 = ORIENTED_EDGE ( 'NONE', *, *, #19283, .F. ) ;
#14587 = ORIENTED_EDGE ( 'NONE', *, *, #11971, .F. ) ;
#14588 = VECTOR ( 'NONE', #1154, 1000.000000000000227 ) ;
#14589 = CARTESIAN_POINT ( 'NONE',  ( 21.25660046192028929, 34.52875999999999834, -13.18703856829094079 ) ) ;
#14590 = AXIS2_PLACEMENT_3D ( 'NONE', #21320, #9489, #21209 ) ;
#14592 = DIRECTION ( 'NONE',  ( 0.000000000000000000, 1.000000000000000000, 0.000000000000000000 ) ) ;
#14591 = CARTESIAN_POINT ( 'NONE',  ( 2.831345877163882196, 20.92518826319738068, 1.835239478882038977 ) ) ;
#14593 = ORIENTED_EDGE ( 'NONE', *, *, #2790, .T. ) ;
#14594 = CARTESIAN_POINT ( 'NONE',  ( 3.878576562893467194, 12.05861442832895669, 0.7413939759094347881 ) ) ;
#14595 = ORIENTED_EDGE ( 'NONE', *, *, #20065, .F. ) ;
#14596 = ORIENTED_EDGE ( 'NONE', *, *, #21779, .T. ) ;
#14597 = EDGE_CURVE ( 'NONE', #14993, #18115, #2357, .T. ) ;
#14598 = ORIENTED_EDGE ( 'NONE', *, *, #5156, .T. ) ;
#14599 = CARTESIAN_POINT ( 'NONE',  ( 2.613241785389884608, 12.04565783673474577, 4.059156808520036464 ) ) ;
#14600 = AXIS2_PLACEMENT_3D ( 'NONE', #2075, #17233, #13386 ) ;
#14601 = CARTESIAN_POINT ( 'NONE',  ( 4.412770401086850924, 11.92270407980696589, 3.040133244938206136 ) ) ;
#14602 = VECTOR ( 'NONE', #4470, 1000.000000000000000 ) ;
#14603 = CARTESIAN_POINT ( 'NONE',  ( 12.91059077353605211, 21.25996874134203907, -21.27604296009081253 ) ) ;
#14604 = CARTESIAN_POINT ( 'NONE',  ( 49.09065990372640442, 30.56064500000000095, -26.70549589918839928 ) ) ;
#14605 = CARTESIAN_POINT ( 'NONE',  ( 59.10939610998308780, 34.52875999999999834, -2.797471275456639539 ) ) ;
#14606 = FACE_OUTER_BOUND ( 'NONE', #21829, .T. ) ;
#14607 = CARTESIAN_POINT ( 'NONE',  ( 3.146901756478003964, 11.73978298677764265, 6.391159807765457224 ) ) ;
#14608 = ORIENTED_EDGE ( 'NONE', *, *, #2912, .T. ) ;
#14609 = CARTESIAN_POINT ( 'NONE',  ( 8.505511374756364873, 36.49567249999999774, -20.97439202360551747 ) ) ;
#14610 = CYLINDRICAL_SURFACE ( 'NONE', #16684, 30.16249999999999076 ) ;
#14611 = DIRECTION ( 'NONE',  ( 0.3928209820863007851, 0.000000000000000000, -0.9196149607486571176 ) ) ;
#14612 = DIRECTION ( 'NONE',  ( 0.000000000000000000, -1.000000000000000000, 0.000000000000000000 ) ) ;
#14613 = DIRECTION ( 'NONE',  ( 0.000000000000000000, -1.000000000000000000, 0.000000000000000000 ) ) ;
#14614 = CIRCLE ( 'NONE', #9275, 30.16249999999998366 ) ;
#14615 = ORIENTED_EDGE ( 'NONE', *, *, #7902, .T. ) ;
#14616 = VERTEX_POINT ( 'NONE', #2469 ) ;
#14617 = CARTESIAN_POINT ( 'NONE',  ( 11.21717328838213135, 19.98250042233096124, -2.706654341015993115 ) ) ;
#14619 = DIRECTION ( 'NONE',  ( 0.08420877549337300871, 0.000000000000000000, 0.9964481331860212121 ) ) ;
#14618 = PLANE ( 'NONE',  #7304 ) ;
#14620 = CARTESIAN_POINT ( 'NONE',  ( 12.10902647966340417, 21.41074805268790371, -1.624989011717251186 ) ) ;
#14621 = ORIENTED_EDGE ( 'NONE', *, *, #19905, .F. ) ;
#14622 = ORIENTED_EDGE ( 'NONE', *, *, #10605, .F. ) ;
#14623 = CARTESIAN_POINT ( 'NONE',  ( -17.46249999999999858, 34.31794000000000011, 0.000000000000000000 ) ) ;
#14624 = CARTESIAN_POINT ( 'NONE',  ( 8.344319702060484900, 21.09743033546479296, -0.3585062597797421535 ) ) ;
#14625 = VECTOR ( 'NONE', #20072, 1000.000000000000227 ) ;
#14626 = CARTESIAN_POINT ( 'NONE',  ( 7.629991675630842352, 20.88079669329302135, 3.443698988702693864 ) ) ;
#14627 = CARTESIAN_POINT ( 'NONE',  ( 6.993352728955766651, 12.42634065549329314, 5.540270479366993683 ) ) ;
#14628 = EDGE_CURVE ( 'NONE', #11489, #5739, #18317, .T. ) ;
#14629 = AXIS2_PLACEMENT_3D ( 'NONE', #1180, #2627, #6257 ) ;
#14630 = DIRECTION ( 'NONE',  ( -0.2490110332224850509, 0.000000000000000000, 0.9685006480810792739 ) ) ;
#14631 = PLANE ( 'NONE',  #19204 ) ;
#14632 = CARTESIAN_POINT ( 'NONE',  ( 38.60701496492545459, 0.000000000000000000, -26.94161103631838472 ) ) ;
#14633 = CARTESIAN_POINT ( 'NONE',  ( 12.59675778470975516, -14.84248999999999974, -12.54640024901842033 ) ) ;
#14634 = CARTESIAN_POINT ( 'NONE',  ( 2.976857449924355858, 19.78000251358870187, 8.006628769824478908 ) ) ;
#14635 = CARTESIAN_POINT ( 'NONE',  ( 1.673502052647580118, 16.21230766891936170, 9.615316047918000208 ) ) ;
#14636 = CIRCLE ( 'NONE', #8953, 5.158739999999998105 ) ;
#14637 = EDGE_LOOP ( 'NONE', ( #1304, #32, #17372, #15485 ) ) ;
#14638 = CARTESIAN_POINT ( 'NONE',  ( 4.104074918077325052, 20.52844081774288298, 5.032055296311012782 ) ) ;
#14639 = DIRECTION ( 'NONE',  ( 0.5087559856598089514, 0.000000000000000000, 0.8609107660235851833 ) ) ;
#14640 = DIRECTION ( 'NONE',  ( 0.000000000000000000, 1.000000000000000000, 0.000000000000000000 ) ) ;
#14641 = CARTESIAN_POINT ( 'NONE',  ( 17.96565374528240611, -7.898429124978179061, -14.43068046346296640 ) ) ;
#14642 = EDGE_LOOP ( 'NONE', ( #8017, #20766, #1191, #2416 ) ) ;
#14643 = CARTESIAN_POINT ( 'NONE',  ( 55.52866846859686234, -1.983739999999999393, -11.12083858657437752 ) ) ;
#14644 = CARTESIAN_POINT ( 'NONE',  ( 9.075928832518638245, 15.79855474736653598, -3.595103111437136345 ) ) ;
#14645 = ORIENTED_EDGE ( 'NONE', *, *, #15539, .F. ) ;
#14646 = AXIS2_PLACEMENT_3D ( 'NONE', #8289, #20312, #1752 ) ;
#14647 = CARTESIAN_POINT ( 'NONE',  ( 20.92131311655350245, -1.145359114192535888, -15.19233952661473097 ) ) ;
#14648 = CARTESIAN_POINT ( 'NONE',  ( 8.218573335227386423, 21.19769852377196173, 5.067010135336594168 ) ) ;
#14649 = LINE ( 'NONE', #12983, #21500 ) ;
#14650 = CARTESIAN_POINT ( 'NONE',  ( 1.515498579774128496, 15.70115217790233508, 8.882780545536347105 ) ) ;
#14651 = ORIENTED_EDGE ( 'NONE', *, *, #6005, .T. ) ;
#14652 = CARTESIAN_POINT ( 'NONE',  ( 67.40134256979101224, 32.54502000000000095, -13.70358117861468017 ) ) ;
#14653 = EDGE_CURVE ( 'NONE', #19435, #15045, #917, .T. ) ;
#14654 = EDGE_CURVE ( 'NONE', #21761, #14134, #9088, .T. ) ;
#14655 = DIRECTION ( 'NONE',  ( 0.9129422336036123742, 0.000000000000000000, -0.4080888115384289083 ) ) ;
#14656 = AXIS2_PLACEMENT_3D ( 'NONE', #11045, #21200, #1083 ) ;
#14657 = CARTESIAN_POINT ( 'NONE',  ( 6.778227844323079232, 11.52015345895104126, 3.130858447466078331 ) ) ;
#14658 = CIRCLE ( 'NONE', #8977, 0.5079999999999993410 ) ;
#14659 = CARTESIAN_POINT ( 'NONE',  ( 70.64340948846358970, 74.97070807199999365, -10.53785647675949910 ) ) ;
#14660 = CARTESIAN_POINT ( 'NONE',  ( 3.633311392490445879, 13.11091270743887982, 8.194468062865079006 ) ) ;
#14661 = CARTESIAN_POINT ( 'NONE',  ( -7.949728765565600597, -7.547927499999999235, -34.47798802950714503 ) ) ;
#14662 = DIRECTION ( 'NONE',  ( 0.000000000000000000, -1.000000000000000000, 0.000000000000000000 ) ) ;
#14663 = CARTESIAN_POINT ( 'NONE',  ( 6.570055536094496773, 11.67239202316484104, 2.792470343458694604 ) ) ;
#14664 = DIRECTION ( 'NONE',  ( 0.000000000000000000, 1.000000000000000000, 0.000000000000000000 ) ) ;
#14665 = DIRECTION ( 'NONE',  ( 0.9579671649362032637, 0.000000000000000000, -0.2868778675745010664 ) ) ;
#14666 = CARTESIAN_POINT ( 'NONE',  ( 19.99312429566830218, 36.51313500000000545, -11.46559883803463720 ) ) ;
#14667 = ORIENTED_EDGE ( 'NONE', *, *, #1561, .F. ) ;
#14668 = LINE ( 'NONE', #19708, #5740 ) ;
#14669 = CIRCLE ( 'NONE', #6168, 0.5080000000000000071 ) ;
#14670 = EDGE_CURVE ( 'NONE', #12461, #14393, #13389, .T. ) ;
#14671 = DIRECTION ( 'NONE',  ( 0.9987059298363657467, 0.000000000000000000, 0.05085730733808445370 ) ) ;
#14672 = ORIENTED_EDGE ( 'NONE', *, *, #4538, .F. ) ;
#14673 = CARTESIAN_POINT ( 'NONE',  ( 11.70990690266660295, 21.06271108513744394, 3.065845505830564477 ) ) ;
#14674 = CARTESIAN_POINT ( 'NONE',  ( -47.86049599909252805, -5.714364999999999029, -23.29373766372935961 ) ) ;
#14675 = CARTESIAN_POINT ( 'NONE',  ( 0.1479864323037562990, 20.14003584071202013, 6.007153626829540904 ) ) ;
#14676 = CARTESIAN_POINT ( 'NONE',  ( 13.89514527990785808, 2.161161825133189218, -15.59098570533049788 ) ) ;
#14677 = CYLINDRICAL_SURFACE ( 'NONE', #18347, 1.190625000000000711 ) ;
#14678 = ORIENTED_EDGE ( 'NONE', *, *, #10570, .T. ) ;
#14679 = SHAPE_REPRESENTATION_RELATIONSHIP ( 'NONE' , 'NONE' ,  #13411, #15909 ) ;
#14680 = AXIS2_PLACEMENT_3D ( 'NONE', #875, #547, #8826 ) ;
#14681 = CARTESIAN_POINT ( 'NONE',  ( 49.16323787629939801, 1.984375000000000000, -27.09503225884920141 ) ) ;
#14682 = ORIENTED_EDGE ( 'NONE', *, *, #9698, .T. ) ;
#14683 = ADVANCED_FACE ( 'NONE', ( #14423, #7662 ), #15865, .T. ) ;
#14684 = CARTESIAN_POINT ( 'NONE',  ( -29.36874999999999858, 1.984375000000000000, 8.335010000000000474 ) ) ;
#14685 = CARTESIAN_POINT ( 'NONE',  ( 17.53610697582018574, -7.943091012973795273, -16.41972336742454530 ) ) ;
#14686 = ORIENTED_EDGE ( 'NONE', *, *, #3422, .T. ) ;
#14687 = CARTESIAN_POINT ( 'NONE',  ( 10.27137985661365960, 20.34432016293438039, 4.929727588585513409 ) ) ;
#14688 = EDGE_CURVE ( 'NONE', #14463, #17254, #10869, .T. ) ;
#14689 = CARTESIAN_POINT ( 'NONE',  ( 38.49809168999158970, 39.83951649598306233, -4.496802017747802083 ) ) ;
#14690 = CARTESIAN_POINT ( 'NONE',  ( 11.95563672222081841, 10.32956393789710070, 0.6582173057821769646 ) ) ;
#14691 = CIRCLE ( 'NONE', #541, 30.16250000000000497 ) ;
#14692 = CARTESIAN_POINT ( 'NONE',  ( 52.50728002481341150, 38.88803500000000213, -18.54895932800084779 ) ) ;
#14693 = DIRECTION ( 'NONE',  ( 0.000000000000000000, 1.000000000000000000, 0.000000000000000000 ) ) ;
#14694 = VERTEX_POINT ( 'NONE', #11193 ) ;
#14695 = LINE ( 'NONE', #2838, #825 ) ;
#14696 = EDGE_CURVE ( 'NONE', #14418, #8481, #15159, .T. ) ;
#14697 = CARTESIAN_POINT ( 'NONE',  ( 17.87574706213523612, -3.968114999999999615, -11.18912023382283571 ) ) ;
#14698 = EDGE_LOOP ( 'NONE', ( #1801, #17665, #4844, #12207 ) ) ;
#14699 = EDGE_CURVE ( 'NONE', #19591, #18990, #1378, .T. ) ;
#14700 = ORIENTED_EDGE ( 'NONE', *, *, #1115, .T. ) ;
#14701 = ADVANCED_FACE ( 'NONE', ( #6104 ), #9313, .F. ) ;
#14702 = CARTESIAN_POINT ( 'NONE',  ( 10.63776237795206825, -4.912495182802602223, -15.95233917191240458 ) ) ;
#14704 = LINE ( 'NONE', #16775, #20860 ) ;
#14703 = CARTESIAN_POINT ( 'NONE',  ( 3.541852216381984331, 16.52290265193734342, 9.336019329946809719 ) ) ;
#14705 = ORIENTED_EDGE ( 'NONE', *, *, #16277, .F. ) ;
#14706 = CARTESIAN_POINT ( 'NONE',  ( 3.742561817426398374, 18.11868962831785268, -1.147007223846213897 ) ) ;
#14707 = ORIENTED_EDGE ( 'NONE', *, *, #18705, .F. ) ;
#14708 = ORIENTED_EDGE ( 'NONE', *, *, #5502, .F. ) ;
#14709 = AXIS2_PLACEMENT_3D ( 'NONE', #12140, #15693, #10469 ) ;
#14710 = ORIENTED_EDGE ( 'NONE', *, *, #15776, .F. ) ;
#14711 = DIRECTION ( 'NONE',  ( -0.2868778675745011220, 0.000000000000000000, -0.9579671649362034858 ) ) ;
#14712 = CARTESIAN_POINT ( 'NONE',  ( 38.18512253410862911, -6.517595172173256124, -4.927479914652646897 ) ) ;
#14713 = CARTESIAN_POINT ( 'NONE',  ( 37.13209340688868565, -6.356984999999999886, -3.529402718062123689 ) ) ;
#14714 = LINE ( 'NONE', #2749, #890 ) ;
#14715 = CARTESIAN_POINT ( 'NONE',  ( 3.002670853353920588, 11.48192359107278193, 5.755866358288438178 ) ) ;
#14716 = ORIENTED_EDGE ( 'NONE', *, *, #14508, .F. ) ;
#14717 = FACE_OUTER_BOUND ( 'NONE', #7597, .T. ) ;
#14718 = CARTESIAN_POINT ( 'NONE',  ( 13.19325985535186874, 21.42039298163480154, 1.900799873352047475 ) ) ;
#14719 = LINE ( 'NONE', #11158, #8200 ) ;
#14720 = EDGE_CURVE ( 'NONE', #9714, #18111, #12547, .T. ) ;
#14721 = CARTESIAN_POINT ( 'NONE',  ( 53.21069847348088189, 40.07865999999999929, -16.58732351464169597 ) ) ;
#14722 = ORIENTED_EDGE ( 'NONE', *, *, #21851, .F. ) ;
#14723 = ADVANCED_FACE ( 'NONE', ( #12431 ), #2793, .F. ) ;
#14724 = ORIENTED_EDGE ( 'NONE', *, *, #10354, .F. ) ;
#14725 = CARTESIAN_POINT ( 'NONE',  ( 13.74851850464161807, 20.92287966070258065, 4.168088350112811646 ) ) ;
#14726 = DIRECTION ( 'NONE',  ( 0.9636276526537417286, 0.000000000000000000, -0.2672484743474500268 ) ) ;
#14727 = CARTESIAN_POINT ( 'NONE',  ( 10.92875438672132127, 14.66671681640350222, -4.110811315144232481 ) ) ;
#14728 = VERTEX_POINT ( 'NONE', #7557 ) ;
#14729 = VERTEX_POINT ( 'NONE', #10977 ) ;
#14730 = DIRECTION ( 'NONE',  ( 0.000000000000000000, 0.000000000000000000, 1.000000000000000000 ) ) ;
#14731 = CARTESIAN_POINT ( 'NONE',  ( 7.582094801143906437, 20.89590603020118209, 3.316103915199458463 ) ) ;
#14732 = CARTESIAN_POINT ( 'NONE',  ( 2.997879949738217142, 18.60940351736496012, 7.792782124073855066 ) ) ;
#14733 = CARTESIAN_POINT ( 'NONE',  ( 1.923689137428217455, 33.48813496001219647, -20.61772871637841220 ) ) ;
#14734 = CARTESIAN_POINT ( 'NONE',  ( -15.40073180482455939, 37.13938632784453375, -10.30507461914819878 ) ) ;
#14735 = CARTESIAN_POINT ( 'NONE',  ( 29.15193331460030279, -7.547927499999999235, -13.61707959051006966 ) ) ;
#14736 = DIRECTION ( 'NONE',  ( 0.000000000000000000, 1.000000000000000000, 0.000000000000000000 ) ) ;
#14737 = CARTESIAN_POINT ( 'NONE',  ( 6.247365411986783634, 10.85645724975988102, 2.357295897773714177 ) ) ;
#14738 = CARTESIAN_POINT ( 'NONE',  ( 1.526806735031254192, 12.95316680106106588, 8.305910411264434856 ) ) ;
#14739 = DIRECTION ( 'NONE',  ( 1.000000000000000000, 0.000000000000000000, 0.000000000000000000 ) ) ;
#14740 = CIRCLE ( 'NONE', #13331, 9.524999999999998579 ) ;
#14741 = ORIENTED_EDGE ( 'NONE', *, *, #1033, .F. ) ;
#14742 = CARTESIAN_POINT ( 'NONE',  ( 1.993078339923719078, 16.41892220718292705, -0.04448763570734674822 ) ) ;
#14743 = CARTESIAN_POINT ( 'NONE',  ( 30.02465935949302533, -5.959792500000001603, -2.324128137548288731 ) ) ;
#14744 = CARTESIAN_POINT ( 'NONE',  ( 53.92488716032378449, -6.193276019600876481, -15.65869747379985988 ) ) ;
#14745 = CARTESIAN_POINT ( 'NONE',  ( 20.42592314637030881, -5.381782642937507077, -13.93043304647089187 ) ) ;
#14746 = ORIENTED_EDGE ( 'NONE', *, *, #7539, .F. ) ;
#14747 = CARTESIAN_POINT ( 'NONE',  ( -23.81250000000000000, 16.27314499999999953, 8.731249999999999289 ) ) ;
#14748 = ADVANCED_FACE ( 'NONE', ( #16297 ), #5967, .T. ) ;
#14749 = CARTESIAN_POINT ( 'NONE',  ( 10.52449966068789600, 21.89451842192714182, 0.08871630297646766750 ) ) ;
#14750 = CARTESIAN_POINT ( 'NONE',  ( 9.098771279194568962, 16.31622443234601505, -3.618126721927819478 ) ) ;
#14751 = ORIENTED_EDGE ( 'NONE', *, *, #11852, .F. ) ;
#14752 = DIRECTION ( 'NONE',  ( 0.2490110332224836354, 0.000000000000000000, -0.9685006480810794960 ) ) ;
#14753 = CARTESIAN_POINT ( 'NONE',  ( 12.86968119689294276, 21.36979473703610211, 0.4932293370143083777 ) ) ;
#14754 = CARTESIAN_POINT ( 'NONE',  ( 7.409109770802898787, 21.71406919359216303, 2.854341070393255464 ) ) ;
#14755 = CARTESIAN_POINT ( 'NONE',  ( 17.30373842852263877, -3.968114999999999615, -12.15706637069277107 ) ) ;
#14756 = CARTESIAN_POINT ( 'NONE',  ( 6.972679700711061024, 18.17742714445450858, 7.378323603228086114 ) ) ;
#14757 = FILL_AREA_STYLE ('',( #16408 ) ) ;
#14758 = CARTESIAN_POINT ( 'NONE',  ( 6.842142561927330391, 18.93559280865479622, 6.839764141372675965 ) ) ;
#14759 = AXIS2_PLACEMENT_3D ( 'NONE', #6615, #21433, #3094 ) ;
#14760 = CARTESIAN_POINT ( 'NONE',  ( 27.87822510359947614, -1.983739999999999837, -8.893823290944665061 ) ) ;
#14761 = CARTESIAN_POINT ( 'NONE',  ( 12.23472727335246546, 21.02863807409008245, 3.597568982022594231 ) ) ;
#14762 = CARTESIAN_POINT ( 'NONE',  ( 5.365249781777944982, 15.79612960646276143, 8.006526335470118383 ) ) ;
#14763 = CARTESIAN_POINT ( 'NONE',  ( -29.36874999999999858, 0.000000000000000000, -3.968750000000000000 ) ) ;
#14764 = CARTESIAN_POINT ( 'NONE',  ( 5.755077836978824024, 17.48971098885959918, 8.606492718269242559 ) ) ;
#14765 = CYLINDRICAL_SURFACE ( 'NONE', #17777, 6.350000000000001421 ) ;
#14766 = CARTESIAN_POINT ( 'NONE',  ( 71.03305177384599745, 0.000000000000000000, -10.93409647675949969 ) ) ;
#14767 = CARTESIAN_POINT ( 'NONE',  ( 6.730216886430935297, 11.15497028527178180, 2.706720253529151687 ) ) ;
#14768 = CARTESIAN_POINT ( 'NONE',  ( 52.49113927203449492, -6.356984999999999886, -16.14695822742181619 ) ) ;
#14769 = CARTESIAN_POINT ( 'NONE',  ( 21.02192561536538307, -1.427578428074376848, -15.15544506753321663 ) ) ;
#14770 = CARTESIAN_POINT ( 'NONE',  ( 12.88040283537677588, 12.29391749999999739, -0.09070320285213756550 ) ) ;
#14771 = EDGE_CURVE ( 'NONE', #7624, #14476, #21136, .T. ) ;
#14772 = ORIENTED_EDGE ( 'NONE', *, *, #7995, .F. ) ;
#14773 = DIRECTION ( 'NONE',  ( 0.9685006480810791629, 0.000000000000000000, 0.2490110332224850231 ) ) ;
#14774 = EDGE_LOOP ( 'NONE', ( #4616, #14438, #12311, #2211 ) ) ;
#14775 = CARTESIAN_POINT ( 'NONE',  ( 9.691931056481777773, 18.84418690367108695, -2.229408216028554435 ) ) ;
#14776 = DIRECTION ( 'NONE',  ( 0.000000000000000000, 1.000000000000000000, 0.000000000000000000 ) ) ;
#14777 = CARTESIAN_POINT ( 'NONE',  ( 52.65905863606531057, 37.83483977376697993, -17.16729226877096792 ) ) ;
#14778 = CARTESIAN_POINT ( 'NONE',  ( 11.91437785957834983, -6.551758114717628700, -15.05791989401956776 ) ) ;
#14780 = CARTESIAN_POINT ( 'NONE',  ( -18.18961309330695997, -3.266559801243759331, -25.80119252674831998 ) ) ;
#14779 = CARTESIAN_POINT ( 'NONE',  ( 6.919136621472420146, 13.22675071421554094, 7.220084409228111788 ) ) ;
#14781 = ORIENTED_EDGE ( 'NONE', *, *, #7706, .F. ) ;
#14782 = CARTESIAN_POINT ( 'NONE',  ( 28.97711086133420366, 1.984375000000000000, -10.31874999999999964 ) ) ;
#14783 = VERTEX_POINT ( 'NONE', #17512 ) ;
#14784 = DIRECTION ( 'NONE',  ( -0.8609107660235849613, 0.000000000000000000, 0.5087559856598092844 ) ) ;
#14785 = CARTESIAN_POINT ( 'NONE',  ( 0.8343063516506451505, 19.60987250044867380, 2.327694854359185772 ) ) ;
#14786 = AXIS2_PLACEMENT_3D ( 'NONE', #5475, #3942, #12130 ) ;
#14787 = VERTEX_POINT ( 'NONE', #15981 ) ;
#14788 = CARTESIAN_POINT ( 'NONE',  ( 7.996957105099447460, 19.55923767994525875, -1.087077586340398971 ) ) ;
#14789 = CARTESIAN_POINT ( 'NONE',  ( 2.535383609039546737, 19.37376392382110168, 1.243470200790914637 ) ) ;
#14790 = EDGE_CURVE ( 'NONE', #1480, #7489, #4126, .T. ) ;
#14791 = CARTESIAN_POINT ( 'NONE',  ( -17.46249999999999858, -1.587500000000002132, 0.000000000000000000 ) ) ;
#14792 = CARTESIAN_POINT ( 'NONE',  ( 11.39967439401671356, 13.68296282620402238, 7.086946939641975973 ) ) ;
#14793 = EDGE_LOOP ( 'NONE', ( #12152, #18875, #4808, #5635 ) ) ;
#14794 = CARTESIAN_POINT ( 'NONE',  ( 20.09810219785228824, -3.122651124923756072, -15.32960905372040017 ) ) ;
#14795 = DIRECTION ( 'NONE',  ( -0.9966381950048638361, 0.000000000000000000, 0.08192867786951606168 ) ) ;
#14796 = EDGE_CURVE ( 'NONE', #966, #14216, #17733, .T. ) ;
#14797 = ORIENTED_EDGE ( 'NONE', *, *, #17784, .T. ) ;
#14798 = ADVANCED_FACE ( 'NONE', ( #4352, #1566 ), #6318, .T. ) ;
#14799 = EDGE_CURVE ( 'NONE', #8773, #2714, #2082, .T. ) ;
#14800 = DIRECTION ( 'NONE',  ( -0.2490110332224850509, 0.000000000000000000, 0.9685006480810792739 ) ) ;
#14801 = CARTESIAN_POINT ( 'NONE',  ( 21.45456921355305724, -14.84248999999999974, -13.95701595352872815 ) ) ;
#14802 = ORIENTED_EDGE ( 'NONE', *, *, #21548, .T. ) ;
#14803 = ORIENTED_EDGE ( 'NONE', *, *, #12249, .F. ) ;
#14804 = VECTOR ( 'NONE', #6242, 1000.000000000000000 ) ;
#14805 = CARTESIAN_POINT ( 'NONE',  ( 14.15750100853548510, -8.464140165015777484, -16.43479104712926642 ) ) ;
#14807 = DIRECTION ( 'NONE',  ( 0.000000000000000000, 1.000000000000000000, 0.000000000000000000 ) ) ;
#14806 = CARTESIAN_POINT ( 'NONE',  ( 2.791956288251989271, 11.23314441701904087, 5.253760342499054659 ) ) ;
#14808 = EDGE_LOOP ( 'NONE', ( #14724, #12591, #19872, #19415 ) ) ;
#14809 = CARTESIAN_POINT ( 'NONE',  ( 3.516109142659268105, 15.63669090343262980, -1.372924135725262396 ) ) ;
#14810 = VERTEX_POINT ( 'NONE', #9743 ) ;
#14811 = ORIENTED_EDGE ( 'NONE', *, *, #18675, .T. ) ;
#14812 = ORIENTED_EDGE ( 'NONE', *, *, #17598, .F. ) ;
#14813 = EDGE_CURVE ( 'NONE', #6814, #1714, #5622, .T. ) ;
#14814 = VECTOR ( 'NONE', #10810, 1000.000000000000000 ) ;
#14815 = DIRECTION ( 'NONE',  ( 0.000000000000000000, 1.000000000000000000, 0.000000000000000000 ) ) ;
#14816 = DIRECTION ( 'NONE',  ( 0.7421532822901579785, 0.000000000000000000, -0.6702301885068630005 ) ) ;
#14817 = CARTESIAN_POINT ( 'NONE',  ( 30.97944403357121956, 32.54502000000000095, -8.103300075789407586 ) ) ;
#14818 = CARTESIAN_POINT ( 'NONE',  ( 1.728940443695251572, 13.74568572289879143, 0.01708573981842225267 ) ) ;
#14819 = VERTEX_POINT ( 'NONE', #16724 ) ;
#14820 = ADVANCED_FACE ( 'NONE', ( #18051 ), #2909, .T. ) ;
#14821 = DIRECTION ( 'NONE',  ( 0.000000000000000000, -1.000000000000000000, 6.254384957144000359E-09 ) ) ;
#14822 = CARTESIAN_POINT ( 'NONE',  ( 30.47347900023190803, 2.586003464000000029, -8.148724574017967015 ) ) ;
#14823 = CARTESIAN_POINT ( 'NONE',  ( 13.09961018545095790, 21.49405002474989601, 1.939654742769484574 ) ) ;
#14824 = VECTOR ( 'NONE', #17615, 1000.000000000000114 ) ;
#14825 = LINE ( 'NONE', #4752, #13400 ) ;
#14826 = ORIENTED_EDGE ( 'NONE', *, *, #11557, .T. ) ;
#14827 = ORIENTED_EDGE ( 'NONE', *, *, #2050, .T. ) ;
#14828 = CARTESIAN_POINT ( 'NONE',  ( 13.55229689020630346, 21.28532635717934340, 3.644360168486233231 ) ) ;
#14829 = DIRECTION ( 'NONE',  ( 0.000000000000000000, -1.000000000000000000, -0.000000000000000000 ) ) ;
#14830 = CARTESIAN_POINT ( 'NONE',  ( 11.34437852127595825, 19.30251821168517878, -3.616633193649956723 ) ) ;
#14831 = ORIENTED_EDGE ( 'NONE', *, *, #5817, .F. ) ;
#14832 = ORIENTED_EDGE ( 'NONE', *, *, #496, .T. ) ;
#14833 = CARTESIAN_POINT ( 'NONE',  ( 26.59062499999999929, 1.984057500000000251, 10.71562499999999929 ) ) ;
#14834 = CARTESIAN_POINT ( 'NONE',  ( 8.250958580417858457, 11.56196078241316094, 2.082770178844938425 ) ) ;
#14835 = CARTESIAN_POINT ( 'NONE',  ( 6.628825292412243719, 11.76599776795001162, 3.880554096689835308 ) ) ;
#14836 = AXIS2_PLACEMENT_3D ( 'NONE', #4152, #16107, #6129 ) ;
#14837 = EDGE_CURVE ( 'NONE', #12265, #5398, #8201, .T. ) ;
#14838 = EDGE_CURVE ( 'NONE', #21482, #5560, #18258, .T. ) ;
#14839 = ADVANCED_FACE ( 'NONE', ( #13202 ), #10077, .F. ) ;
#14840 = CARTESIAN_POINT ( 'NONE',  ( -17.01419847615277092, 34.52875999999999834, -25.90052557009608236 ) ) ;
#14841 = CARTESIAN_POINT ( 'NONE',  ( 44.27024749654656688, -6.356984999999999886, -8.722764363618033201 ) ) ;
#14842 = FACE_OUTER_BOUND ( 'NONE', #425, .T. ) ;
#14843 = CARTESIAN_POINT ( 'NONE',  ( 17.02725982432203367, -1.983739999999999393, -14.27444360421403857 ) ) ;
#14844 = CARTESIAN_POINT ( 'NONE',  ( 2.786917533582454531, 20.92456416987101875, 1.848867324536296319 ) ) ;
#14845 = CARTESIAN_POINT ( 'NONE',  ( 1.702540419714505981, 15.43467393698043111, 9.533519331230623450 ) ) ;
#14846 = DIRECTION ( 'NONE',  ( -1.000000000000000000, 0.000000000000000000, 0.000000000000000000 ) ) ;
#14847 = ORIENTED_EDGE ( 'NONE', *, *, #17803, .F. ) ;
#14848 = CARTESIAN_POINT ( 'NONE',  ( 4.906036559996388213, 12.10288835339510172, 5.342054952800848966 ) ) ;
#14849 = CARTESIAN_POINT ( 'NONE',  ( 38.82016491058538321, 0.000000000000000000, -14.75770094105646812 ) ) ;
#14850 = CARTESIAN_POINT ( 'NONE',  ( -21.43124999999999858, 30.56064500000000095, -4.860316984116058095E-16 ) ) ;
#14851 = CARTESIAN_POINT ( 'NONE',  ( 20.35416303201372301, -5.534383657676722024, -13.94270872964028563 ) ) ;
#14852 = ORIENTED_EDGE ( 'NONE', *, *, #1564, .T. ) ;
#14853 = CARTESIAN_POINT ( 'NONE',  ( 9.739256322687126044, 10.74433361426668121, 0.2283133401813704499 ) ) ;
#14854 = CIRCLE ( 'NONE', #19063, 0.7950199999999982836 ) ;
#14855 = CARTESIAN_POINT ( 'NONE',  ( 9.112690981491565978, 16.57506450310666324, -3.621295390223508548 ) ) ;
#14856 = ORIENTED_EDGE ( 'NONE', *, *, #1803, .T. ) ;
#14857 = AXIS2_PLACEMENT_3D ( 'NONE', #10994, #17858, #2704 ) ;
#14858 = CARTESIAN_POINT ( 'NONE',  ( 7.074389910882576515, 21.61684822571231024, 1.935217957262916455 ) ) ;
#14859 = LINE ( 'NONE', #9967, #17279 ) ;
#14860 = CARTESIAN_POINT ( 'NONE',  ( 3.855364176784159991, 12.82285234092424098, 0.9140719758827169361 ) ) ;
#14861 = CARTESIAN_POINT ( 'NONE',  ( 32.42378190387104553, -1.983739999999999837, -18.15178106273469183 ) ) ;
#14862 = AXIS2_PLACEMENT_3D ( 'NONE', #17590, #17919, #11168 ) ;
#14863 = CARTESIAN_POINT ( 'NONE',  ( 32.52436584422698473, 0.000000000000000000, 1.884807767196291284 ) ) ;
#14864 = EDGE_CURVE ( 'NONE', #8797, #4861, #3230, .T. ) ;
#14865 = CARTESIAN_POINT ( 'NONE',  ( 9.537190736074361297, 15.40389167150912009, -3.043062899500690754 ) ) ;
#14866 = AXIS2_PLACEMENT_3D ( 'NONE', #581, #5660, #354 ) ;
#14867 = AXIS2_PLACEMENT_3D ( 'NONE', #6228, #6334, #12891 ) ;
#14868 = CARTESIAN_POINT ( 'NONE',  ( -0.5435003404963313356, 3.961447500000001565, -25.80650133522849998 ) ) ;
#14869 = CARTESIAN_POINT ( 'NONE',  ( 5.429893219852483632, 19.16583807351516100, 7.915143928656239503 ) ) ;
#14870 = DIRECTION ( 'NONE',  ( -0.2227372614607789347, 0.000000000000000000, -0.9748785115884710528 ) ) ;
#14871 = CARTESIAN_POINT ( 'NONE',  ( 28.87608719841374949, 2.770822500000000854, -15.73691681567849976 ) ) ;
#14872 = LINE ( 'NONE', #19603, #13586 ) ;
#14873 = DIRECTION ( 'NONE',  ( 0.2227372614607789347, 0.000000000000000000, 0.9748785115884710528 ) ) ;
#14874 = CARTESIAN_POINT ( 'NONE',  ( 21.24317407479450281, -2.610281063246285616, -15.05445591060229660 ) ) ;
#14875 = DIRECTION ( 'NONE',  ( 0.000000000000000000, 1.000000000000000000, 0.000000000000000000 ) ) ;
#14876 = VECTOR ( 'NONE', #4760, 1000.000000000000000 ) ;
#14877 = ORIENTED_EDGE ( 'NONE', *, *, #6926, .F. ) ;
#14878 = LINE ( 'NONE', #6124, #13519 ) ;
#14879 = CIRCLE ( 'NONE', #3208, 9.525000000000000355 ) ;
#14880 = CARTESIAN_POINT ( 'NONE',  ( 3.360635606688116894, -14.84248999999999974, -20.45316710734507026 ) ) ;
#14881 = ORIENTED_EDGE ( 'NONE', *, *, #2574, .F. ) ;
#14882 = CARTESIAN_POINT ( 'NONE',  ( 13.04011110611221191, 17.29791255147096862, 6.322173244565231442 ) ) ;
#14883 = DIRECTION ( 'NONE',  ( 0.08420877549337300871, 0.000000000000000000, 0.9964481331860212121 ) ) ;
#14884 = CARTESIAN_POINT ( 'NONE',  ( 19.50372870060111552, -0.8007013868912387089, -15.11219580267691143 ) ) ;
#14886 = DIRECTION ( 'NONE',  ( -0.1132953773954069460, 0.7241889112991807265, -0.6802312681817409556 ) ) ;
#14885 = CARTESIAN_POINT ( 'NONE',  ( 5.614794017493704104, 11.64278443974904320, 1.417881410066428094 ) ) ;
#14887 = ORIENTED_EDGE ( 'NONE', *, *, #17879, .T. ) ;
#14888 = CARTESIAN_POINT ( 'NONE',  ( 0.000000000000000000, 0.000000000000000000, 0.000000000000000000 ) ) ;
#14889 = AXIS2_PLACEMENT_3D ( 'NONE', #14666, #18274, #9758 ) ;
#14890 = LINE ( 'NONE', #19618, #1790 ) ;
#14891 = DIRECTION ( 'NONE',  ( 0.000000000000000000, -1.000000000000000000, -0.000000000000000000 ) ) ;
#14892 = EDGE_LOOP ( 'NONE', ( #12781, #20080, #16987, #16224 ) ) ;
#14893 = CARTESIAN_POINT ( 'NONE',  ( 19.71456874936146875, -0.4919948594096015815, -14.92276603756576492 ) ) ;
#14894 = VECTOR ( 'NONE', #10658, 1000.000000000000000 ) ;
#14895 = ADVANCED_FACE ( 'NONE', ( #11745 ), #4881, .F. ) ;
#14896 = AXIS2_PLACEMENT_3D ( 'NONE', #11450, #19834, #8011 ) ;
#14897 = CARTESIAN_POINT ( 'NONE',  ( 20.50301314505018624, -0.3073934294499542919, -15.81860185314828016 ) ) ;
#14898 = ORIENTED_EDGE ( 'NONE', *, *, #8968, .F. ) ;
#14899 = CARTESIAN_POINT ( 'NONE',  ( 8.986932461157417507, 18.23310434598736052, 6.953159659984535779 ) ) ;
#14900 = CARTESIAN_POINT ( 'NONE',  ( 2.969052100254564674, 20.17138864544537569, 2.328491213132350079 ) ) ;
#14901 = AXIS2_PLACEMENT_3D ( 'NONE', #10793, #2273, #2386 ) ;
#14902 = DIRECTION ( 'NONE',  ( 0.000000000000000000, 1.000000000000000000, 0.000000000000000000 ) ) ;
#14903 = CARTESIAN_POINT ( 'NONE',  ( 13.40212049016752083, 14.65538885420913573, 7.066582115483678095 ) ) ;
#14904 = EDGE_CURVE ( 'NONE', #9456, #7901, #1453, .T. ) ;
#14905 = CIRCLE ( 'NONE', #21581, 11.02160133116777985 ) ;
#14906 = CARTESIAN_POINT ( 'NONE',  ( -17.46249999999999858, 0.000000000000000000, 0.000000000000000000 ) ) ;
#14907 = EDGE_LOOP ( 'NONE', ( #11186, #18774 ) ) ;
#14908 = CARTESIAN_POINT ( 'NONE',  ( 9.720932288844398528, 20.95102166027618296, 3.388999603248170178 ) ) ;
#14909 = CARTESIAN_POINT ( 'NONE',  ( 9.441987842462824077, 11.74734702153278043, -1.584992358009425839 ) ) ;
#14910 = DIRECTION ( 'NONE',  ( 0.000000000000000000, 1.000000000000000000, 0.000000000000000000 ) ) ;
#14911 = VECTOR ( 'NONE', #20135, 1000.000000000000000 ) ;
#14912 = ORIENTED_EDGE ( 'NONE', *, *, #21707, .T. ) ;
#14913 = ORIENTED_EDGE ( 'NONE', *, *, #11971, .T. ) ;
#14914 = AXIS2_PLACEMENT_3D ( 'NONE', #2660, #2876, #14391 ) ;
#14915 = CARTESIAN_POINT ( 'NONE',  ( 29.76562500000000000, 32.54502000000000095, -4.317999999999999616 ) ) ;
#14916 = CARTESIAN_POINT ( 'NONE',  ( 0.6728160834238413601, 11.31186333555498180, 4.884450196609837924 ) ) ;
#14917 = ORIENTED_EDGE ( 'NONE', *, *, #18010, .T. ) ;
#14918 = CARTESIAN_POINT ( 'NONE',  ( 4.548213313756960474, 20.72542134385079393, 0.8261887588110893299 ) ) ;
#14919 = EDGE_CURVE ( 'NONE', #5923, #3431, #8084, .T. ) ;
#14920 = ORIENTED_EDGE ( 'NONE', *, *, #13340, .T. ) ;
#14921 = ORIENTED_EDGE ( 'NONE', *, *, #2624, .F. ) ;
#14922 = CARTESIAN_POINT ( 'NONE',  ( 1.156505235941993837, 12.68153838805022104, 6.702054009790849420 ) ) ;
#14923 = EDGE_CURVE ( 'NONE', #16893, #18301, #14859, .T. ) ;
#14924 = CARTESIAN_POINT ( 'NONE',  ( 14.05820270259704152, -3.968114999999999615, -15.03781736451272444 ) ) ;
#14925 = VERTEX_POINT ( 'NONE', #13405 ) ;
#14926 = EDGE_CURVE ( 'NONE', #20877, #17636, #16822, .T. ) ;
#14927 = AXIS2_PLACEMENT_3D ( 'NONE', #9804, #14931, #18224 ) ;
#14928 = CARTESIAN_POINT ( 'NONE',  ( 13.69372857911114671, 14.67906862019266612, 6.891448972015076002 ) ) ;
#14929 = CIRCLE ( 'NONE', #3972, 1.785937499999999956 ) ;
#14930 = CARTESIAN_POINT ( 'NONE',  ( 4.499766462069353601, 11.88009950761181166, 3.431268433568689602 ) ) ;
#14931 = DIRECTION ( 'NONE',  ( 0.000000000000000000, 1.000000000000000000, 0.000000000000000000 ) ) ;
#14932 = DIRECTION ( 'NONE',  ( 0.2227372614607789347, 0.000000000000000000, 0.9748785115884710528 ) ) ;
#14933 = CARTESIAN_POINT ( 'NONE',  ( 62.90077106633562209, 36.51313500000000545, 8.141649473166729933 ) ) ;
#14934 = CARTESIAN_POINT ( 'NONE',  ( 2.164828507489252374, 19.30256671482680275, 0.1920966893002172826 ) ) ;
#14935 = AXIS2_PLACEMENT_3D ( 'NONE', #16260, #2986, #1206 ) ;
#14936 = ORIENTED_EDGE ( 'NONE', *, *, #13178, .F. ) ;
#14937 = DIRECTION ( 'NONE',  ( 0.000000000000000000, -1.000000000000000000, 0.000000000000000000 ) ) ;
#14938 = DIRECTION ( 'NONE',  ( 0.2868778675745011220, 0.000000000000000000, 0.9579671649362034858 ) ) ;
#14939 = LINE ( 'NONE', #3088, #17334 ) ;
#14940 = CARTESIAN_POINT ( 'NONE',  ( 53.49467103128933587, 39.92874023264636207, -16.24638064876058507 ) ) ;
#14941 = ORIENTED_EDGE ( 'NONE', *, *, #14720, .T. ) ;
#14942 = ORIENTED_EDGE ( 'NONE', *, *, #8042, .F. ) ;
#14943 = CARTESIAN_POINT ( 'NONE',  ( 7.239715322470854808, 21.09291897731618093, 3.289218189963096339 ) ) ;
#14944 = DIRECTION ( 'NONE',  ( 0.9579671649362032637, 0.000000000000000000, -0.2868778675745010664 ) ) ;
#14945 = ORIENTED_EDGE ( 'NONE', *, *, #12659, .F. ) ;
#14946 = ADVANCED_FACE ( 'NONE', ( #6212 ), #14975, .F. ) ;
#14947 = VERTEX_POINT ( 'NONE', #7872 ) ;
#14948 = FACE_OUTER_BOUND ( 'NONE', #1650, .T. ) ;
#14949 = CARTESIAN_POINT ( 'NONE',  ( 9.250817896104313931, 14.36852381253967259, 6.813382293121613920 ) ) ;
#14950 = VECTOR ( 'NONE', #7020, 1000.000000000000114 ) ;
#14951 = AXIS2_PLACEMENT_3D ( 'NONE', #17295, #16098, #19278 ) ;
#14952 = EDGE_CURVE ( 'NONE', #17422, #4597, #14649, .T. ) ;
#14953 = CARTESIAN_POINT ( 'NONE',  ( 3.238746979964965078, 17.52814199671485440, 8.277643969343714048 ) ) ;
#14954 = AXIS2_PLACEMENT_3D ( 'NONE', #16996, #13697, #13592 ) ;
#14955 = EDGE_CURVE ( 'NONE', #10206, #7846, #13309, .T. ) ;
#14956 = DIRECTION ( 'NONE',  ( 0.000000000000000000, -1.000000000000000000, -0.000000000000000000 ) ) ;
#14957 = LINE ( 'NONE', #21671, #13609 ) ;
#14958 = CARTESIAN_POINT ( 'NONE',  ( 0.3397968550407932109, 11.79551702397467672, 3.001928043112756406 ) ) ;
#14959 = DIRECTION ( 'NONE',  ( 0.000000000000000000, 1.000000000000000000, 0.000000000000000000 ) ) ;
#14960 = ORIENTED_EDGE ( 'NONE', *, *, #8174, .F. ) ;
#14961 = CARTESIAN_POINT ( 'NONE',  ( 4.565292852930672218, 11.78113229454884170, 3.809678802701250699 ) ) ;
#14962 = DIRECTION ( 'NONE',  ( 0.8583349619704310207, 0.000000000000000000, -0.5130897514657826175 ) ) ;
#14963 = DIRECTION ( 'NONE',  ( 0.2490110332224850509, 0.000000000000000000, -0.9685006480810792739 ) ) ;
#14964 = CARTESIAN_POINT ( 'NONE',  ( 13.67320413129362677, -8.014437261679972835, -15.36892139067619212 ) ) ;
#14965 = ORIENTED_EDGE ( 'NONE', *, *, #5550, .T. ) ;
#14966 = CARTESIAN_POINT ( 'NONE',  ( 7.345424518500083266, 18.37388711802374530, -2.636412766723661871 ) ) ;
#14967 = CIRCLE ( 'NONE', #18454, 0.7950200000000000600 ) ;
#14968 = DIRECTION ( 'NONE',  ( -0.5733392046337749681, 0.8193181045417647912, 0.000000000000000000 ) ) ;
#14969 = CARTESIAN_POINT ( 'NONE',  ( 9.360979028382789835, 12.15336758057035738, -1.848830518539319678 ) ) ;
#14970 = VERTEX_POINT ( 'NONE', #9639 ) ;
#14971 = EDGE_CURVE ( 'NONE', #9393, #3115, #13407, .T. ) ;
#14972 = EDGE_CURVE ( 'NONE', #20317, #8304, #14981, .T. ) ;
#14973 = ADVANCED_FACE ( 'NONE', ( #16305 ), #1140, .T. ) ;
#14974 = CARTESIAN_POINT ( 'NONE',  ( 6.036247796095363327, 19.98418368318813165, -0.8363276938606165611 ) ) ;
#14975 = PLANE ( 'NONE',  #20084 ) ;
#14976 = CARTESIAN_POINT ( 'NONE',  ( 0.2144152073732452368, 13.13615472609876100, 2.170878085811235092 ) ) ;
#14977 = CARTESIAN_POINT ( 'NONE',  ( 30.33489826846160398, 30.56064500000000095, -2.417033907079745525 ) ) ;
#14978 = VECTOR ( 'NONE', #17985, 1000.000000000000000 ) ;
#14979 = DIRECTION ( 'NONE',  ( -0.000000000000000000, -1.000000000000000000, 0.000000000000000000 ) ) ;
#14980 = ORIENTED_EDGE ( 'NONE', *, *, #20702, .F. ) ;
#14981 = LINE ( 'NONE', #6219, #1034 ) ;
#14982 = AXIS2_PLACEMENT_3D ( 'NONE', #4843, #11581, #8684 ) ;
#14983 = CARTESIAN_POINT ( 'NONE',  ( 11.57888104933464746, 12.79277479448814248, -2.537844513231963361 ) ) ;
#14984 = CARTESIAN_POINT ( 'NONE',  ( 32.55306802826559220, 32.54502000000000095, -17.37731658638881527 ) ) ;
#14985 = CARTESIAN_POINT ( 'NONE',  ( 7.796181282232575782, 16.63782405840064982, 8.320680270861050332 ) ) ;
#14986 = LINE ( 'NONE', #15415, #10002 ) ;
#14987 = CARTESIAN_POINT ( 'NONE',  ( -17.46249999999999858, -1.983740000000001169, 0.000000000000000000 ) ) ;
#14988 = CARTESIAN_POINT ( 'NONE',  ( 6.555793388040663139, 10.96622957324827219, 2.745169609115350351 ) ) ;
#14989 = LINE ( 'NONE', #21704, #9370 ) ;
#14990 = CARTESIAN_POINT ( 'NONE',  ( 20.92131311655350245, -1.145359114192535888, -15.19233952661473097 ) ) ;
#14991 = AXIS2_PLACEMENT_3D ( 'NONE', #14841, #14511, #6087 ) ;
#14992 = CYLINDRICAL_SURFACE ( 'NONE', #7445, 25.00312499999999361 ) ;
#14993 = VERTEX_POINT ( 'NONE', #6324 ) ;
#14994 = CARTESIAN_POINT ( 'NONE',  ( 43.29176983217143260, 2.586003464000000029, 5.154088326438659884 ) ) ;
#14995 = DIRECTION ( 'NONE',  ( -0.8667647648559581031, 0.000000000000000000, -0.4987171968201974948 ) ) ;
#14996 = DIRECTION ( 'NONE',  ( 0.000000000000000000, 0.000000000000000000, 1.000000000000000000 ) ) ;
#14997 = EDGE_CURVE ( 'NONE', #2625, #19416, #16244, .T. ) ;
#14998 = CARTESIAN_POINT ( 'NONE',  ( 12.55379232897500152, 19.58114513849477234, 5.265243977356697691 ) ) ;
#14999 = DIRECTION ( 'NONE',  ( -0.000000000000000000, -1.000000000000000000, 0.000000000000000000 ) ) ;
#15000 = DIRECTION ( 'NONE',  ( -0.9685006480810792739, 0.000000000000000000, -0.2490110332224846346 ) ) ;
#15001 = CARTESIAN_POINT ( 'NONE',  ( 12.32505589497316478, -0.5459407413539660858, -16.45354645552742667 ) ) ;
#15002 = DIRECTION ( 'NONE',  ( 0.7334850928793759106, 0.6768732144311037091, -0.06198604769977157647 ) ) ;
#15003 = VERTEX_POINT ( 'NONE', #16512 ) ;
#15004 = DIRECTION ( 'NONE',  ( 0.1060008583745199739, 0.000000000000000000, 0.9943660382494290406 ) ) ;
#15005 = CARTESIAN_POINT ( 'NONE',  ( 4.131751249095085399, 18.64349594346743189, -0.07007902096679233250 ) ) ;
#15006 = LINE ( 'NONE', #15107, #3844 ) ;
#15007 = EDGE_LOOP ( 'NONE', ( #12975, #14832, #20467, #7126 ) ) ;
#15008 = CARTESIAN_POINT ( 'NONE',  ( 27.40895291499714403, 34.52875999999999834, -9.088367920799473865 ) ) ;
#15009 = CARTESIAN_POINT ( 'NONE',  ( 14.32880508193474256, -8.336696740575057163, -16.92443569652990476 ) ) ;
#15010 = ORIENTED_EDGE ( 'NONE', *, *, #3587, .T. ) ;
#15011 = B_SPLINE_CURVE_WITH_KNOTS ( 'NONE', 3,
 ( #338, #15621, #460, #18681 ),
 .UNSPECIFIED., .F., .F.,
 ( 4, 4 ),
 ( 0.000000000000000000, 1.000000000000000000 ),
 .UNSPECIFIED. ) ;
#15012 = CARTESIAN_POINT ( 'NONE',  ( 9.316412786783502042, 13.73224064219962592, -2.236872125683732282 ) ) ;
#15013 = CARTESIAN_POINT ( 'NONE',  ( 5.315127011898622023, 15.44490212850582189, -2.184099619210333909 ) ) ;
#15014 = AXIS2_PLACEMENT_3D ( 'NONE', #19695, #9748, #14427 ) ;
#15015 = CARTESIAN_POINT ( 'NONE',  ( 17.19146193903594977, -7.054867240447602050, -15.83036007852367533 ) ) ;
#15016 = CARTESIAN_POINT ( 'NONE',  ( 13.11799571124250363, 13.08957250000000094, -19.78847697788343396 ) ) ;
#15017 = ORIENTED_EDGE ( 'NONE', *, *, #319, .F. ) ;
#15018 = CARTESIAN_POINT ( 'NONE',  ( 9.652372407212508776, 20.99368581358743313, 3.205678883041131577 ) ) ;
#15019 = CARTESIAN_POINT ( 'NONE',  ( 13.12356091339558262, 18.81087267297494137, 6.763476435230526107 ) ) ;
#15020 = DIRECTION ( 'NONE',  ( 0.000000000000000000, 0.000000000000000000, -1.000000000000000000 ) ) ;
#15021 = ORIENTED_EDGE ( 'NONE', *, *, #3446, .T. ) ;
#15022 = VERTEX_POINT ( 'NONE', #9428 ) ;
#15023 = ADVANCED_FACE ( 'NONE', ( #9749 ), #13208, .F. ) ;
#15024 = CARTESIAN_POINT ( 'NONE',  ( -53.00154558624916490, -14.84248999999999974, -22.85927301266823264 ) ) ;
#15026 = CARTESIAN_POINT ( 'NONE',  ( -1.345424459097947834, 12.30439499999999953, 2.648158502653860324 ) ) ;
#15025 = CARTESIAN_POINT ( 'NONE',  ( 3.586014194197774785, 14.72191889613304205, 9.088953234725488883 ) ) ;
#15027 = ORIENTED_EDGE ( 'NONE', *, *, #11149, .F. ) ;
#15028 = CARTESIAN_POINT ( 'NONE',  ( 5.598095257095291544, 21.53640102163099357, 3.667698324075315153 ) ) ;
#15029 = ORIENTED_EDGE ( 'NONE', *, *, #18624, .T. ) ;
#15030 = ORIENTED_EDGE ( 'NONE', *, *, #1803, .F. ) ;
#15031 = CARTESIAN_POINT ( 'NONE',  ( 0.3666840790735627076, 12.67405468869563201, 2.999742210112375851 ) ) ;
#15032 = EDGE_CURVE ( 'NONE', #19233, #16242, #8522, .T. ) ;
#15033 = DIRECTION ( 'NONE',  ( 0.000000000000000000, 0.000000000000000000, 1.000000000000000000 ) ) ;
#15034 = ORIENTED_EDGE ( 'NONE', *, *, #7506, .F. ) ;
#15035 = CIRCLE ( 'NONE', #9354, 0.7950200000000005041 ) ;
#15036 = CARTESIAN_POINT ( 'NONE',  ( 5.498548077612729124, 13.58815257356176076, -1.570838218170207856 ) ) ;
#15037 = CARTESIAN_POINT ( 'NONE',  ( -23.01875000000000071, 30.56064500000000095, -10.31874999999999964 ) ) ;
#15038 = FACE_OUTER_BOUND ( 'NONE', #418, .T. ) ;
#15039 = CARTESIAN_POINT ( 'NONE',  ( 2.355781047999157884, 19.88761438775357604, 0.6622465411279562231 ) ) ;
#15040 = ORIENTED_EDGE ( 'NONE', *, *, #21825, .F. ) ;
#15041 = CARTESIAN_POINT ( 'NONE',  ( 53.84486179190094646, 42.06303499999999929, -6.412645463410259872 ) ) ;
#15042 = CARTESIAN_POINT ( 'NONE',  ( 42.27821610176829381, 32.54502000000000095, 7.496956594510385763 ) ) ;
#15043 = DIRECTION ( 'NONE',  ( -0.6702301885068630005, 0.000000000000000000, -0.7421532822901579785 ) ) ;
#15044 = CARTESIAN_POINT ( 'NONE',  ( 13.67756757867809725, 32.52628750000000224, 2.571257636385987144 ) ) ;
#15045 = VERTEX_POINT ( 'NONE', #6647 ) ;
#15046 = EDGE_LOOP ( 'NONE', ( #13018, #20918, #16756, #8207, #8013, #17139, #8054, #6889, #9467, #9114, #16236, #14051 ) ) ;
#15047 = EDGE_CURVE ( 'NONE', #11999, #6050, #18481, .T. ) ;
#15048 = CARTESIAN_POINT ( 'NONE',  ( 6.027233423144887858, 11.87704527764502060, 1.641552790826397157 ) ) ;
#15049 = ADVANCED_FACE ( 'NONE', ( #10416 ), #5108, .T. ) ;
#15051 = DIRECTION ( 'NONE',  ( 0.9964481331860213231, 0.000000000000000000, -0.08420877549337293932 ) ) ;
#15050 = DIRECTION ( 'NONE',  ( -0.1060008583745224581, 0.000000000000000000, -0.9943660382494288186 ) ) ;
#15052 = VERTEX_POINT ( 'NONE', #6978 ) ;
#15053 = AXIS2_PLACEMENT_3D ( 'NONE', #11102, #8914, #12888 ) ;
#15054 = ORIENTED_EDGE ( 'NONE', *, *, #16578, .T. ) ;
#15055 = CARTESIAN_POINT ( 'NONE',  ( 52.65345379380355695, 37.69740999999999786, -16.29354262597941982 ) ) ;
#15056 = ORIENTED_EDGE ( 'NONE', *, *, #12352, .T. ) ;
#15057 = CARTESIAN_POINT ( 'NONE',  ( 8.234567635551437448, 11.56963249381149161, 2.010831876170865229 ) ) ;
#15058 = CARTESIAN_POINT ( 'NONE',  ( 6.732418519251836209, 11.87159243078942161, 4.343617615359864459 ) ) ;
#15059 = CARTESIAN_POINT ( 'NONE',  ( 3.089332131768892431, 18.26930023550903925, 7.991679757977339094 ) ) ;
#15060 = EDGE_CURVE ( 'NONE', #12232, #21727, #3353, .T. ) ;
#15061 = CARTESIAN_POINT ( 'NONE',  ( -7.949728765565600597, 33.32892749999999893, -34.47798802950714503 ) ) ;
#15062 = DIRECTION ( 'NONE',  ( -0.9790635044817342925, 0.000000000000000000, 0.2035550397114870846 ) ) ;
#15063 = CARTESIAN_POINT ( 'NONE',  ( 0.4154230101138479681, 19.55300952260564173, 1.162825123489284573 ) ) ;
#15064 = CARTESIAN_POINT ( 'NONE',  ( 24.43309469626978725, 9.340595522457139310, -0.6496488801123181389 ) ) ;
#15065 = ORIENTED_EDGE ( 'NONE', *, *, #5055, .T. ) ;
#15066 = CARTESIAN_POINT ( 'NONE',  ( 3.676953213723906710, 13.56078169262926281, 7.585074204264090625 ) ) ;
#15067 = CYLINDRICAL_SURFACE ( 'NONE', #6049, 25.00312499999999361 ) ;
#15068 = CARTESIAN_POINT ( 'NONE',  ( 14.33584040382675262, 6.343967500000000648, -46.84351661546690337 ) ) ;
#15069 =( NAMED_UNIT ( * ) PLANE_ANGLE_UNIT ( ) SI_UNIT ( $, .RADIAN. ) );
#15070 = CARTESIAN_POINT ( 'NONE',  ( -12.61651652020322523, -1.587500000000002132, -1.064728033956553244 ) ) ;
#15071 = ORIENTED_EDGE ( 'NONE', *, *, #8101, .T. ) ;
#15072 = EDGE_CURVE ( 'NONE', #7901, #17335, #20885, .T. ) ;
#15073 = CARTESIAN_POINT ( 'NONE',  ( 9.133094369329063156, 11.81448552380872208, -1.435243799284318111 ) ) ;
#15074 = EDGE_CURVE ( 'NONE', #3974, #11144, #17993, .T. ) ;
#15075 = CARTESIAN_POINT ( 'NONE',  ( 9.997327980603063935, 20.80492458171390169, -1.606069075083376374 ) ) ;
#15076 = ORIENTED_EDGE ( 'NONE', *, *, #13717, .T. ) ;
#15077 = CARTESIAN_POINT ( 'NONE',  ( 9.194614005794997880, 18.51609980883254991, 7.549505974447304091 ) ) ;
#15078 = DIRECTION ( 'NONE',  ( 1.000000000000000000, 0.000000000000000000, 0.000000000000000000 ) ) ;
#15079 = CARTESIAN_POINT ( 'NONE',  ( 39.42154620619644589, -7.547609999999999708, -4.343957374020581241 ) ) ;
#15080 = DIRECTION ( 'NONE',  ( -0.000000000000000000, -1.000000000000000000, 0.000000000000000000 ) ) ;
#15081 = DIRECTION ( 'NONE',  ( 0.000000000000000000, 1.000000000000000000, 0.000000000000000000 ) ) ;
#15082 = CARTESIAN_POINT ( 'NONE',  ( 26.41404040124396602, 30.54508749999999750, -1.242873262350622010 ) ) ;
#15083 = VECTOR ( 'NONE', #660, 1000.000000000000114 ) ;
#15084 = CARTESIAN_POINT ( 'NONE',  ( 5.990136806399605440, 17.32712159277285124, -1.922517228740736384 ) ) ;
#15085 = CARTESIAN_POINT ( 'NONE',  ( 5.254588850512410758, 13.39928225704216658, 6.969322526385836269 ) ) ;
#15086 = EDGE_CURVE ( 'NONE', #21482, #7846, #1397, .T. ) ;
#15087 = CARTESIAN_POINT ( 'NONE',  ( 1.819498930146989046, 15.58835493759099400, 9.633805599351241256 ) ) ;
#15088 = DIRECTION ( 'NONE',  ( 0.9685006480810794960, 0.000000000000000000, 0.2490110332224836354 ) ) ;
#15089 = DIRECTION ( 'NONE',  ( -0.9579671649362034858, 0.000000000000000000, 0.2868778675745011220 ) ) ;
#15090 = CARTESIAN_POINT ( 'NONE',  ( 2.075021368115900877, 17.94205954657215685, 0.2607137428604667795 ) ) ;
#15091 = FACE_OUTER_BOUND ( 'NONE', #7373, .T. ) ;
#15092 = CARTESIAN_POINT ( 'NONE',  ( 19.13395524456137053, -7.364572356485500570, -15.39828872268818927 ) ) ;
#15093 = DIRECTION ( 'NONE',  ( 0.000000000000000000, 1.000000000000000000, 0.000000000000000000 ) ) ;
#15094 = ORIENTED_EDGE ( 'NONE', *, *, #7913, .T. ) ;
#15095 = LINE ( 'NONE', #21809, #4687 ) ;
#15096 = CARTESIAN_POINT ( 'NONE',  ( 21.05324281572633538, -1.171894783154180164, -15.19005319227003525 ) ) ;
#15097 = LINE ( 'NONE', #13426, #14911 ) ;
#15098 = CARTESIAN_POINT ( 'NONE',  ( 13.16336969972371485, 15.65847078906175049, 6.372932858607479822 ) ) ;
#15099 = PLANE ( 'NONE',  #9172 ) ;
#15100 = AXIS2_PLACEMENT_3D ( 'NONE', #5922, #10910, #14356 ) ;
#15101 = CARTESIAN_POINT ( 'NONE',  ( 52.38908862829682533, 38.14157091315900061, -17.41777910622722914 ) ) ;
#15102 = CARTESIAN_POINT ( 'NONE',  ( 11.03537156866804025, -4.708219523321687916, -15.20365171484573708 ) ) ;
#15103 = CARTESIAN_POINT ( 'NONE',  ( 5.772535574092870547, 11.93222000202738187, 1.495588789165622545 ) ) ;
#15104 = ORIENTED_EDGE ( 'NONE', *, *, #7193, .T. ) ;
#15105 =( NAMED_UNIT ( * ) SI_UNIT ( $, .STERADIAN. ) SOLID_ANGLE_UNIT ( ) );
#15106 = CARTESIAN_POINT ( 'NONE',  ( -15.39353573898878658, -4.587157632697119958, -10.30107656633069979 ) ) ;
#15107 = CARTESIAN_POINT ( 'NONE',  ( 39.11079947626275555, 32.54502000000000095, -27.65534212225540500 ) ) ;
#15108 = CARTESIAN_POINT ( 'NONE',  ( 6.220337769557592544, 11.67239398284132257, 2.897195776018576918 ) ) ;
#15109 = CARTESIAN_POINT ( 'NONE',  ( 21.08655736082664944, -1.169157187581218338, -15.28996091734704699 ) ) ;
#15110 = ORIENTED_EDGE ( 'NONE', *, *, #1891, .T. ) ;
#15111 = CARTESIAN_POINT ( 'NONE',  ( 12.84446185305211685, 21.48375758380098333, 0.5023101645198579934 ) ) ;
#15112 = EDGE_CURVE ( 'NONE', #4078, #1509, #17710, .T. ) ;
#15113 = CARTESIAN_POINT ( 'NONE',  ( 11.25866438965172556, 15.74982258328167717, 6.880959276425811844 ) ) ;
#15114 = DIRECTION ( 'NONE',  ( 0.000000000000000000, 1.000000000000000000, 0.000000000000000000 ) ) ;
#15115 = ADVANCED_FACE ( 'NONE', ( #3783 ), #20676, .T. ) ;
#15116 = CARTESIAN_POINT ( 'NONE',  ( 9.388584069342069682, 11.74734702153278043, -1.568999784240643125 ) ) ;
#15117 = VECTOR ( 'NONE', #15392, 1000.000000000000000 ) ;
#15118 = CARTESIAN_POINT ( 'NONE',  ( 13.05392461046280417, -5.983512873707068636, -16.67921711117497097 ) ) ;
#15119 = DIRECTION ( 'NONE',  ( 0.4987171968201974948, 0.000000000000000000, -0.8667647648559582141 ) ) ;
#15120 = ORIENTED_EDGE ( 'NONE', *, *, #8143, .T. ) ;
#15121 = CARTESIAN_POINT ( 'NONE',  ( 8.296946464115761088, 20.10878641201166772, -0.3926114842361396184 ) ) ;
#15122 = CARTESIAN_POINT ( 'NONE',  ( 9.251884976597745336, 18.56541443352003640, 7.643588779325639848 ) ) ;
#15123 = EDGE_LOOP ( 'NONE', ( #16153, #18793, #1954, #4946 ) ) ;
#15124 = ORIENTED_EDGE ( 'NONE', *, *, #437, .F. ) ;
#15125 = CARTESIAN_POINT ( 'NONE',  ( 32.17043356788648367, 34.52875999999999834, -17.71146456218788146 ) ) ;
#15127 = CARTESIAN_POINT ( 'NONE',  ( 52.80360533369807285, 37.69740999999999786, -16.43086303210407451 ) ) ;
#15126 = CARTESIAN_POINT ( 'NONE',  ( -0.3109692073693477443, 15.59583246595391692, 0.02116780168869621809 ) ) ;
#15128 = ORIENTED_EDGE ( 'NONE', *, *, #17854, .F. ) ;
#15129 = CARTESIAN_POINT ( 'NONE',  ( 4.995330526685626715, 21.31046569428566073, 2.024587815778703614 ) ) ;
#15130 = AXIS2_PLACEMENT_3D ( 'NONE', #3104, #21673, #13296 ) ;
#15131 = ORIENTED_EDGE ( 'NONE', *, *, #2574, .T. ) ;
#15132 = CARTESIAN_POINT ( 'NONE',  ( 0.4679875273695434101, 12.45726290459096219, 3.483910897087822089 ) ) ;
#15133 = CARTESIAN_POINT ( 'NONE',  ( 44.27024749654656688, -9.531985000000000596, -8.722764363618033201 ) ) ;
#15134 = ORIENTED_EDGE ( 'NONE', *, *, #6248, .T. ) ;
#15135 = CARTESIAN_POINT ( 'NONE',  ( 2.071751749769342510, 13.12036018483466648, 1.505555561256101127 ) ) ;
#15136 = ADVANCED_FACE ( 'NONE', ( #5534 ), #4006, .T. ) ;
#15137 = DIRECTION ( 'NONE',  ( 1.000000000000000000, 0.000000000000000000, 0.000000000000000000 ) ) ;
#15138 = CARTESIAN_POINT ( 'NONE',  ( 39.00487391863466513, 40.07742955315917044, -3.894748490060887747 ) ) ;
#15139 = CARTESIAN_POINT ( 'NONE',  ( 2.602153466714682839, 20.45502326233802393, 1.293897402751491565 ) ) ;
#15140 = AXIS2_PLACEMENT_3D ( 'NONE', #7312, #15954, #12290 ) ;
#15141 = VERTEX_POINT ( 'NONE', #7093 ) ;
#15142 = CARTESIAN_POINT ( 'NONE',  ( 59.86950051480232560, -6.356984999999999886, -17.89453710146031185 ) ) ;
#15143 = LINE ( 'NONE', #13164, #64 ) ;
#15144 = CARTESIAN_POINT ( 'NONE',  ( 39.62791084302666178, 34.52875999999999834, -24.65774797299118859 ) ) ;
#15145 = LINE ( 'NONE', #13480, #6051 ) ;
#15146 = DIRECTION ( 'NONE',  ( 0.9987059298363656357, 0.000000000000000000, 0.05085730733808393328 ) ) ;
#15147 = ORIENTED_EDGE ( 'NONE', *, *, #705, .T. ) ;
#15148 = ORIENTED_EDGE ( 'NONE', *, *, #2365, .F. ) ;
#15149 = CARTESIAN_POINT ( 'NONE',  ( 8.107474665427385929, 11.49260726995666104, 1.880968186788171792 ) ) ;
#15150 = CARTESIAN_POINT ( 'NONE',  ( -13.57684171658811678, 0.000000000000000000, -0.8078590638549644209 ) ) ;
#15151 = ORIENTED_EDGE ( 'NONE', *, *, #4185, .F. ) ;
#15152 = ORIENTED_EDGE ( 'NONE', *, *, #17760, .T. ) ;
#15153 = LINE ( 'NONE', #4645, #6377 ) ;
#15154 = ORIENTED_EDGE ( 'NONE', *, *, #9623, .F. ) ;
#15155 = CARTESIAN_POINT ( 'NONE',  ( 8.981279084499066201, 12.48120098075682805, 5.346287112963081789 ) ) ;
#15156 = VECTOR ( 'NONE', #14891, 1000.000000000000000 ) ;
#15157 = ADVANCED_FACE ( 'NONE', ( #17387, #4653, #11072 ), #18144, .F. ) ;
#15158 = LINE ( 'NONE', #13499, #18702 ) ;
#15159 = CIRCLE ( 'NONE', #5612, 1.190625000000001155 ) ;
#15160 = DIRECTION ( 'NONE',  ( -0.4128958666089267981, 0.5884034904305870395, 0.6951966166390379787 ) ) ;
#15161 = CARTESIAN_POINT ( 'NONE',  ( 46.07940063401251507, 0.000000000000000000, -26.08707253294707229 ) ) ;
#15162 = CARTESIAN_POINT ( 'NONE',  ( 0.05081553632030246653, 12.65820550866425620, 1.671469819115525723 ) ) ;
#15163 = DIRECTION ( 'NONE',  ( -0.9579671649362033747, 0.000000000000000000, 0.2868778675745011220 ) ) ;
#15164 = VERTEX_POINT ( 'NONE', #6296 ) ;
#15165 = CARTESIAN_POINT ( 'NONE',  ( 6.767590535262720586, 11.71523883824356282, 4.062906024995755594 ) ) ;
#15166 = CARTESIAN_POINT ( 'NONE',  ( 65.90927232300019512, 32.54502000000000095, -13.30734117861468135 ) ) ;
#15167 = CARTESIAN_POINT ( 'NONE',  ( 17.79723720954694954, -3.968114999999999615, -14.07647485258271303 ) ) ;
#15168 = DIRECTION ( 'NONE',  ( 0.000000000000000000, 1.000000000000000000, 0.000000000000000000 ) ) ;
#15169 = LINE ( 'NONE', #1444, #7003 ) ;
#15170 = ORIENTED_EDGE ( 'NONE', *, *, #18053, .T. ) ;
#15171 = CARTESIAN_POINT ( 'NONE',  ( 13.09788092753539424, 14.67906862019266612, 7.069884632380020406 ) ) ;
#15172 = AXIS2_PLACEMENT_3D ( 'NONE', #10279, #17028, #15399 ) ;
#15173 = DIRECTION ( 'NONE',  ( -0.9685006480810792739, 0.000000000000000000, -0.2490110332224846346 ) ) ;
#15174 = CARTESIAN_POINT ( 'NONE',  ( 11.32645464201832652, 22.04042062782242084, 2.039904004311749564 ) ) ;
#15175 = ORIENTED_EDGE ( 'NONE', *, *, #6381, .T. ) ;
#15176 = CIRCLE ( 'NONE', #5676, 0.7950200000000005041 ) ;
#15177 = CARTESIAN_POINT ( 'NONE',  ( 8.523675650794778846, 10.78766231307313994, 3.249609201625923927 ) ) ;
#15178 = CARTESIAN_POINT ( 'NONE',  ( 3.167498170806753777, 12.59169734781732330, 6.476231790880818018 ) ) ;
#15179 = CARTESIAN_POINT ( 'NONE',  ( 48.78323016782857735, 2.586003464000000029, -25.79158832643865651 ) ) ;
#15180 = EDGE_CURVE ( 'NONE', #5796, #18451, #4541, .T. ) ;
#15181 = CARTESIAN_POINT ( 'NONE',  ( 7.254584665336054172, 16.67580702288875116, 7.619632138345714623 ) ) ;
#15182 = LINE ( 'NONE', #5105, #6523 ) ;
#15183 = ADVANCED_FACE ( 'NONE', ( #18027 ), #16383, .T. ) ;
#15184 = CARTESIAN_POINT ( 'NONE',  ( 54.78059207134182884, -6.356984999999999886, -16.96151288338074181 ) ) ;
#15185 = CARTESIAN_POINT ( 'NONE',  ( 11.61973461185466583, 18.13781435472470349, -3.585029466117453989 ) ) ;
#15186 = EDGE_CURVE ( 'NONE', #11827, #13842, #19752, .T. ) ;
#15187 = CARTESIAN_POINT ( 'NONE',  ( 3.613208712544091039, 16.52268874363389628, 9.310180084879426943 ) ) ;
#15188 = CARTESIAN_POINT ( 'NONE',  ( 28.38195592936287781, -7.547927499999999235, -13.81504834214261024 ) ) ;
#15189 = CARTESIAN_POINT ( 'NONE',  ( 19.99297611413309639, -0.4553737095896724374, -14.82343000113548648 ) ) ;
#15190 = AXIS2_PLACEMENT_3D ( 'NONE', #7857, #1325, #1112 ) ;
#15191 = CARTESIAN_POINT ( 'NONE',  ( 3.161989770655216248, 17.96135795615357011, 8.230302926828514387 ) ) ;
#15192 = DIRECTION ( 'NONE',  ( -0.7421532822901579785, 0.000000000000000000, 0.6702301885068628895 ) ) ;
#15193 = DIRECTION ( 'NONE',  ( 0.000000000000000000, 1.000000000000000000, 0.000000000000000000 ) ) ;
#15194 = CARTESIAN_POINT ( 'NONE',  ( 12.35968435821843947, -6.936577703317105659, -16.86437037943348116 ) ) ;
#15195 = DIRECTION ( 'NONE',  ( -0.9579671649362032637, 0.000000000000000000, 0.2868778675745010664 ) ) ;
#15196 = ORIENTED_EDGE ( 'NONE', *, *, #14300, .F. ) ;
#15197 = DIRECTION ( 'NONE',  ( 0.000000000000000000, 1.000000000000000000, -0.000000000000000000 ) ) ;
#15198 = CARTESIAN_POINT ( 'NONE',  ( 9.699109564081849655, 21.77551566733012933, 3.361061402723362512 ) ) ;
#15199 = VERTEX_POINT ( 'NONE', #16171 ) ;
#15200 = CARTESIAN_POINT ( 'NONE',  ( 12.83002304812085015, 12.17901403585384656, 4.356414321884917840 ) ) ;
#15201 = CARTESIAN_POINT ( 'NONE',  ( -23.01875000000000071, 0.000000000000000000, -3.968750000000000000 ) ) ;
#15202 = CARTESIAN_POINT ( 'NONE',  ( 11.60004900376628711, -3.656864654387723679, -15.55631684518033886 ) ) ;
#15203 = CARTESIAN_POINT ( 'NONE',  ( 3.505934377962688586, 17.20635281421107265, -0.6812542612677440212 ) ) ;
#15204 = ORIENTED_EDGE ( 'NONE', *, *, #11902, .T. ) ;
#15205 = EDGE_CURVE ( 'NONE', #3064, #20432, #997, .T. ) ;
#15206 = LINE ( 'NONE', #21821, #17353 ) ;
#15207 = CARTESIAN_POINT ( 'NONE',  ( 13.62051399351888747, 17.23237496650334677, -17.80340391586448234 ) ) ;
#15208 = AXIS2_PLACEMENT_3D ( 'NONE', #19361, #7228, #10755 ) ;
#15209 = CARTESIAN_POINT ( 'NONE',  ( 6.206257128763711606, 10.96622738556230026, 2.849852413749992763 ) ) ;
#15210 = CIRCLE ( 'NONE', #12018, 0.5953125000000004663 ) ;
#15211 = ORIENTED_EDGE ( 'NONE', *, *, #15611, .F. ) ;
#15212 = CARTESIAN_POINT ( 'NONE',  ( 8.098296366812832048, 20.59418330540166053, 4.742484706917446502 ) ) ;
#15213 = ADVANCED_FACE ( 'NONE', ( #3530 ), #16705, .F. ) ;
#15214 = CARTESIAN_POINT ( 'NONE',  ( 9.685017632263924980, 18.90675885874853890, -2.319252428474684269 ) ) ;
#15215 = CARTESIAN_POINT ( 'NONE',  ( 6.658090509130313528, 20.81351436963172219, 5.254839933866528590 ) ) ;
#15216 = CARTESIAN_POINT ( 'NONE',  ( 13.55166441465202176, 22.20239475586336297, 2.436989766962892823 ) ) ;
#15217 = AXIS2_PLACEMENT_3D ( 'NONE', #20094, #16485, #1319 ) ;
#15218 = CARTESIAN_POINT ( 'NONE',  ( 16.12778039609075265, -7.242576738085929833, -16.05200023831469025 ) ) ;
#15219 = DIRECTION ( 'NONE',  ( -0.9685006480810792739, 0.000000000000000000, -0.2490110332224846346 ) ) ;
#15220 = EDGE_LOOP ( 'NONE', ( #14941, #19477, #9874, #3200 ) ) ;
#15221 = AXIS2_PLACEMENT_3D ( 'NONE', #1717, #1506, #3288 ) ;
#15222 = CARTESIAN_POINT ( 'NONE',  ( 10.83319469175927985, 18.70694946134396375, 6.220917748816447990 ) ) ;
#15223 = CARTESIAN_POINT ( 'NONE',  ( 12.95755072449374090, 11.26929059074382167, 4.630978755562344062 ) ) ;
#15224 = CIRCLE ( 'NONE', #7793, 30.16249999999999076 ) ;
#15225 = ORIENTED_EDGE ( 'NONE', *, *, #20281, .F. ) ;
#15226 = ORIENTED_EDGE ( 'NONE', *, *, #13736, .T. ) ;
#15227 = DIRECTION ( 'NONE',  ( 1.000000000000000000, 0.000000000000000000, 0.000000000000000000 ) ) ;
#15228 = CARTESIAN_POINT ( 'NONE',  ( 11.05480056376844544, 17.56817812073120422, -4.236062988348112235 ) ) ;
#15230 = CARTESIAN_POINT ( 'NONE',  ( 17.85969298310271114, 1.982787499999999481, 1.318856445756055873 ) ) ;
#15229 = CARTESIAN_POINT ( 'NONE',  ( 1.361757355601472597, 13.96208391574584162, 9.123754984142934177 ) ) ;
#15231 = ORIENTED_EDGE ( 'NONE', *, *, #7195, .F. ) ;
#15232 = CARTESIAN_POINT ( 'NONE',  ( 5.936085032262425010, 21.40849574231920371, 4.589919153110645134 ) ) ;
#15233 = EDGE_CURVE ( 'NONE', #3189, #5229, #13420, .T. ) ;
#15234 = MECHANICAL_DESIGN_GEOMETRIC_PRESENTATION_REPRESENTATION (  '', ( #20 ), #7448 ) ;
#15235 = EDGE_CURVE ( 'NONE', #2495, #4521, #11642, .T. ) ;
#15236 = LINE ( 'NONE', #5150, #6639 ) ;
#15237 = ADVANCED_FACE ( 'NONE', ( #8383 ), #9945, .F. ) ;
#15238 = CIRCLE ( 'NONE', #5000, 0.7950200000000003930 ) ;
#15239 = ORIENTED_EDGE ( 'NONE', *, *, #19826, .F. ) ;
#15240 = AXIS2_PLACEMENT_3D ( 'NONE', #8031, #14807, #11572 ) ;
#15241 = CARTESIAN_POINT ( 'NONE',  ( 0.5565784135784356268, 12.32463844299294209, 3.900071968666352973 ) ) ;
#15242 = FACE_OUTER_BOUND ( 'NONE', #6868, .T. ) ;
#15243 = ORIENTED_EDGE ( 'NONE', *, *, #7613, .F. ) ;
#15244 = AXIS2_PLACEMENT_3D ( 'NONE', #11085, #804, #4016 ) ;
#15245 = CARTESIAN_POINT ( 'NONE',  ( 3.788814298098374778, 14.00384518420827185, -0.003950202559398034718 ) ) ;
#15246 = DIRECTION ( 'NONE',  ( 0.000000000000000000, -1.000000000000000000, -0.000000000000000000 ) ) ;
#15247 = FACE_OUTER_BOUND ( 'NONE', #13366, .T. ) ;
#15248 = CARTESIAN_POINT ( 'NONE',  ( -13.87568970999206108, 34.52875999999999834, -9.457638332870221376 ) ) ;
#15249 = CARTESIAN_POINT ( 'NONE',  ( 2.872526310428787699, 20.88929092507290264, 2.007101110068493899 ) ) ;
#15250 = FACE_OUTER_BOUND ( 'NONE', #9386, .T. ) ;
#15251 = VECTOR ( 'NONE', #11164, 1000.000000000000114 ) ;
#15252 = ORIENTED_EDGE ( 'NONE', *, *, #19260, .F. ) ;
#15253 = B_SPLINE_CURVE_WITH_KNOTS ( 'NONE', 3,
 ( #9304, #7755, #14521, #1331, #13080, #16078, #908, #11081 ),
 .UNSPECIFIED., .F., .F.,
 ( 4, 2, 2, 4 ),
 ( 0.000000000000000000, 0.4999999999999966693, 0.7499999999999983347, 1.000000000000000000 ),
 .UNSPECIFIED. ) ;
#15254 = CARTESIAN_POINT ( 'NONE',  ( 30.50878709810603340, 34.52875999999999834, -19.83971405306587954 ) ) ;
#15255 = CARTESIAN_POINT ( 'NONE',  ( -21.73672411175306962, 33.73373999999999739, 0.8886449702404600748 ) ) ;
#15256 = DIRECTION ( 'NONE',  ( 0.9876802608827760510, 0.000000000000000000, -0.1564854698127960131 ) ) ;
#15257 = DIRECTION ( 'NONE',  ( 0.000000000000000000, -1.000000000000000000, -0.000000000000000000 ) ) ;
#15259 = CARTESIAN_POINT ( 'NONE',  ( 13.04319607734463382, -6.245671925844710870, -15.47036368354625147 ) ) ;
#15258 = LINE ( 'NONE', #13700, #18321 ) ;
#15260 = ORIENTED_EDGE ( 'NONE', *, *, #4417, .F. ) ;
#15261 = VERTEX_POINT ( 'NONE', #6851 ) ;
#15262 = CIRCLE ( 'NONE', #5351, 9.524999999999998579 ) ;
#15263 = CARTESIAN_POINT ( 'NONE',  ( 7.332841212239828543, 14.65140826333467139, -1.889360907835787584 ) ) ;
#15265 = DIRECTION ( 'NONE',  ( 0.000000000000000000, 1.000000000000000000, 0.000000000000000000 ) ) ;
#15264 = CARTESIAN_POINT ( 'NONE',  ( 1.622819991010447493, 17.33683664400565050, 9.603356706031211942 ) ) ;
#15266 = ORIENTED_EDGE ( 'NONE', *, *, #13217, .F. ) ;
#15267 = ORIENTED_EDGE ( 'NONE', *, *, #11245, .T. ) ;
#15268 = EDGE_CURVE ( 'NONE', #5196, #7695, #15158, .T. ) ;
#15269 = FACE_OUTER_BOUND ( 'NONE', #9441, .T. ) ;
#15270 = ORIENTED_EDGE ( 'NONE', *, *, #2449, .F. ) ;
#15271 = CARTESIAN_POINT ( 'NONE',  ( 9.162049469916118127, 13.41167720919363582, 6.257157424146843283 ) ) ;
#15272 = AXIS2_PLACEMENT_3D ( 'NONE', #10065, #10399, #8504 ) ;
#15273 = AXIS2_PLACEMENT_3D ( 'NONE', #12034, #3750, #10483 ) ;
#15274 = CARTESIAN_POINT ( 'NONE',  ( 3.384545484207448496, 16.33714236856847535, 8.445044841043495509 ) ) ;
#15275 = VECTOR ( 'NONE', #4426, 1000.000000000000000 ) ;
#15276 = CARTESIAN_POINT ( 'NONE',  ( 31.02798609601340729, -1.983739999999999837, -5.485920235548950252 ) ) ;
#15277 = CIRCLE ( 'NONE', #14935, 0.7950200000000003930 ) ;
#15278 = CARTESIAN_POINT ( 'NONE',  ( 1.268730000000000135, 9.129395000000000593, 8.609509071587499562 ) ) ;
#15279 = DIRECTION ( 'NONE',  ( 0.9876802608827758290, 0.000000000000000000, -0.1564854698127972066 ) ) ;
#15280 = CARTESIAN_POINT ( 'NONE',  ( 0.5341928495527494825, 19.88375074128939346, 1.456988048183946560 ) ) ;
#15281 = DIRECTION ( 'NONE',  ( 0.000000000000000000, -1.000000000000000000, -0.000000000000000000 ) ) ;
#15282 = ORIENTED_EDGE ( 'NONE', *, *, #10432, .F. ) ;
#15283 = CARTESIAN_POINT ( 'NONE',  ( 5.292371360443332229, 12.95486688907394246, 6.632903289465746255 ) ) ;
#15284 = CARTESIAN_POINT ( 'NONE',  ( 32.55306802826559220, -1.983739999999999837, -17.37731658638881527 ) ) ;
#15285 = CARTESIAN_POINT ( 'NONE',  ( 53.10651001381376091, -7.547610000000002373, -16.70269254552787075 ) ) ;
#15286 = CARTESIAN_POINT ( 'NONE',  ( 8.011380105705496746, -6.752907499999998286, -19.05252355006962617 ) ) ;
#15287 = VECTOR ( 'NONE', #5001, 1000.000000000000000 ) ;
#15288 = ORIENTED_EDGE ( 'NONE', *, *, #1811, .F. ) ;
#15289 = CARTESIAN_POINT ( 'NONE',  ( 5.059806928477906141, 15.45793682862229801, -2.017440984236586576 ) ) ;
#15290 = FACE_OUTER_BOUND ( 'NONE', #9585, .T. ) ;
#15291 = CARTESIAN_POINT ( 'NONE',  ( 13.34013785991228573, 16.63357698718011690, 7.165916878433363557 ) ) ;
#15292 = ORIENTED_EDGE ( 'NONE', *, *, #2816, .T. ) ;
#15293 = ORIENTED_EDGE ( 'NONE', *, *, #735, .F. ) ;
#15294 = EDGE_CURVE ( 'NONE', #10693, #18449, #11832, .T. ) ;
#15295 = CIRCLE ( 'NONE', #8212, 4.961572499999999941 ) ;
#15296 = CARTESIAN_POINT ( 'NONE',  ( 8.408550922056784671, 10.74106511205577164, 2.765873773487825815 ) ) ;
#15297 = AXIS2_PLACEMENT_3D ( 'NONE', #17907, #14612, #17808 ) ;
#15298 = CARTESIAN_POINT ( 'NONE',  ( 7.026614297195842518, 12.34350287060300211, 5.586514903065737947 ) ) ;
#15299 = DIRECTION ( 'NONE',  ( 0.1065921516619544457, 0.9937903127262237568, -0.03192064434796798578 ) ) ;
#15300 = CARTESIAN_POINT ( 'NONE',  ( 7.172396199599091027, 17.36778504101753740, 7.516626074145736247 ) ) ;
#15301 = DIRECTION ( 'NONE',  ( -0.2490110332224850231, 0.000000000000000000, 0.9685006480810791629 ) ) ;
#15302 = AXIS2_PLACEMENT_3D ( 'NONE', #14308, #17602, #9076 ) ;
#15303 = CARTESIAN_POINT ( 'NONE',  ( 11.89439084632494215, 11.62217351343478278, -1.089731598560132575 ) ) ;
#15304 = CARTESIAN_POINT ( 'NONE',  ( 2.651964239740473683, 16.26393749999999727, 5.873042593501262232 ) ) ;
#15305 = CARTESIAN_POINT ( 'NONE',  ( -0.9181641814394345680, 20.56338889613970267, 3.252949121733808457 ) ) ;
#15306 = DIRECTION ( 'NONE',  ( 0.2868778675745010664, 0.000000000000000000, 0.9579671649362032637 ) ) ;
#15307 = VECTOR ( 'NONE', #14085, 1000.000000000000000 ) ;
#15308 = CARTESIAN_POINT ( 'NONE',  ( 19.77720994532765530, -0.02498380418638844122, -14.87308496498962818 ) ) ;
#15309 = CARTESIAN_POINT ( 'NONE',  ( 3.372374456746679350, 16.48230391985759979, 8.538301946733126258 ) ) ;
#15310 = DIRECTION ( 'NONE',  ( -0.9966381950048638361, 0.000000000000000000, 0.08192867786951606168 ) ) ;
#15311 = CARTESIAN_POINT ( 'NONE',  ( 14.65205695078418380, -8.252331693867256845, -16.37421283785102233 ) ) ;
#15312 = CARTESIAN_POINT ( 'NONE',  ( 30.02465935949302533, 39.28268749999999443, -2.324128137548288731 ) ) ;
#15313 = ORIENTED_EDGE ( 'NONE', *, *, #15345, .T. ) ;
#15314 = PLANE ( 'NONE',  #10326 ) ;
#15315 = CARTESIAN_POINT ( 'NONE',  ( 10.97450655955806198, 19.34169052257783505, 6.746375022551643674 ) ) ;
#15316 = DIRECTION ( 'NONE',  ( 0.9685006480810792739, -0.000000000000000000, 0.2490110332224850509 ) ) ;
#15317 = AXIS2_PLACEMENT_3D ( 'NONE', #16202, #9850, #1027 ) ;
#15318 = LINE ( 'NONE', #21713, #11718 ) ;
#15319 = EDGE_CURVE ( 'NONE', #18275, #5609, #4596, .T. ) ;
#15320 = CARTESIAN_POINT ( 'NONE',  ( 12.99318388508481092, 12.89692632477686551, 5.134509715740512625 ) ) ;
#15321 = EDGE_CURVE ( 'NONE', #9160, #10315, #5647, .T. ) ;
#15322 = CARTESIAN_POINT ( 'NONE',  ( 6.585898268469219552, 0.000000000000000000, 4.694966092919240275 ) ) ;
#15323 = CARTESIAN_POINT ( 'NONE',  ( 3.179746087645565211, 14.94275550331619229, 8.487434319128327687 ) ) ;
#15324 = ORIENTED_EDGE ( 'NONE', *, *, #8819, .F. ) ;
#15325 = CARTESIAN_POINT ( 'NONE',  ( -0.6062791574742081302, 20.63358940807441400, 5.277116226863125092 ) ) ;
#15326 = DIRECTION ( 'NONE',  ( -0.3447671952293630548, 0.000000000000000000, -0.9386882235831439658 ) ) ;
#15327 = AXIS2_PLACEMENT_3D ( 'NONE', #8738, #7316, #345 ) ;
#15328 = CARTESIAN_POINT ( 'NONE',  ( 6.288799001572192182, 11.69884688535491080, 2.878624824896528267 ) ) ;
#15329 = CARTESIAN_POINT ( 'NONE',  ( 11.68026082588236747, -6.323616958189365533, -17.48499852013087974 ) ) ;
#15330 = ORIENTED_EDGE ( 'NONE', *, *, #1587, .T. ) ;
#15331 = CARTESIAN_POINT ( 'NONE',  ( 5.664688483032882083, 17.24315932450417321, -1.411349549249473645 ) ) ;
#15332 = CARTESIAN_POINT ( 'NONE',  ( 3.192747775439045199, 20.40795131746391533, 2.906160320096165428 ) ) ;
#15333 = CARTESIAN_POINT ( 'NONE',  ( 11.03274821853219478, 12.61666159072338189, 5.337489519850219466 ) ) ;
#15334 = CARTESIAN_POINT ( 'NONE',  ( 4.291439396447429111, 12.50969690204968288, 0.5082001374855064091 ) ) ;
#15335 = CARTESIAN_POINT ( 'NONE',  ( 12.82184179453522255, 22.28580575005450370, 0.3944390745095269213 ) ) ;
#15336 = EDGE_CURVE ( 'NONE', #2932, #6593, #7417, .T. ) ;
#15337 = DIRECTION ( 'NONE',  ( 0.000000000000000000, 1.000000000000000000, 0.000000000000000000 ) ) ;
#15338 = EDGE_LOOP ( 'NONE', ( #1391, #1637, #19785, #3602, #5918, #11037, #3754, #8023, #13505, #5618, #9861, #586, #11286, #10686, #12260, #3164, #12840, #7655, #13248, #12043, #11417 ) ) ;
#15339 = CARTESIAN_POINT ( 'NONE',  ( 11.06256098204447902, 17.48602064462742334, 6.685474825520898889 ) ) ;
#15340 = CARTESIAN_POINT ( 'NONE',  ( 10.81007580454433281, 10.89927089225536250, 4.167050900241501488 ) ) ;
#15341 = ORIENTED_EDGE ( 'NONE', *, *, #11108, .T. ) ;
#15342 = ORIENTED_EDGE ( 'NONE', *, *, #19537, .T. ) ;
#15343 = FACE_OUTER_BOUND ( 'NONE', #18073, .T. ) ;
#15344 = DIRECTION ( 'NONE',  ( -0.000000000000000000, -1.000000000000000000, 0.000000000000000000 ) ) ;
#15345 = EDGE_CURVE ( 'NONE', #11015, #16300, #9173, .T. ) ;
#15347 = CARTESIAN_POINT ( 'NONE',  ( 31.68988926855799448, -1.983739999999999837, 1.626235259850384418 ) ) ;
#15346 = CARTESIAN_POINT ( 'NONE',  ( 2.000949203156153544, 19.75183458472020348, 0.6057391540848391376 ) ) ;
#15348 = ORIENTED_EDGE ( 'NONE', *, *, #14813, .F. ) ;
#15349 = CARTESIAN_POINT ( 'NONE',  ( 6.702764444734650162, 20.32026046638254613, 6.637863228519256253 ) ) ;
#15350 = AXIS2_PLACEMENT_3D ( 'NONE', #6953, #16806, #20873 ) ;
#15351 = CARTESIAN_POINT ( 'NONE',  ( -22.90596259062238005, 41.43438499999999891, -9.869321627248080375 ) ) ;
#15352 = ORIENTED_EDGE ( 'NONE', *, *, #7195, .T. ) ;
#15353 = ADVANCED_FACE ( 'NONE', ( #12555 ), #4138, .T. ) ;
#15354 = CARTESIAN_POINT ( 'NONE',  ( 13.64200589084435578, -6.754812500000002551, -0.3187768451312169571 ) ) ;
#15355 = VERTEX_POINT ( 'NONE', #21699 ) ;
#15356 = AXIS2_PLACEMENT_3D ( 'NONE', #9319, #16410, #6112 ) ;
#15357 = CARTESIAN_POINT ( 'NONE',  ( 3.851420698079342841, 13.47177213679970720, 0.3669712269455133735 ) ) ;
#15358 = LINE ( 'NONE', #8364, #6441 ) ;
#15359 = DIRECTION ( 'NONE',  ( -0.2035550397114870846, 0.000000000000000000, -0.9790635044817342925 ) ) ;
#15360 = EDGE_CURVE ( 'NONE', #15052, #11891, #6326, .T. ) ;
#15361 = VECTOR ( 'NONE', #2027, 1000.000000000000000 ) ;
#15362 = PRODUCT_DEFINITION_SHAPE ( 'NONE', 'NONE',  #21884 ) ;
#15363 = CARTESIAN_POINT ( 'NONE',  ( -15.61825442841647593, 37.36444197669704437, -10.42024638160073735 ) ) ;
#15364 = CARTESIAN_POINT ( 'NONE',  ( 3.436124513232142519, 21.34046060373059106, 3.525057534639083556 ) ) ;
#15365 = EDGE_CURVE ( 'NONE', #227, #6968, #13316, .T. ) ;
#15366 = CYLINDRICAL_SURFACE ( 'NONE', #14050, 1.983740000000001391 ) ;
#15367 = EDGE_CURVE ( 'NONE', #7181, #7389, #19811, .T. ) ;
#15368 = ORIENTED_EDGE ( 'NONE', *, *, #20746, .T. ) ;
#15369 = LINE ( 'NONE', #10701, #4355 ) ;
#15370 = DIRECTION ( 'NONE',  ( 0.9685006480810792739, 0.000000000000000000, 0.2490110332224850509 ) ) ;
#15371 = CARTESIAN_POINT ( 'NONE',  ( 13.28822531734660828, 34.52875999999999834, -15.23578611614444078 ) ) ;
#15373 = CARTESIAN_POINT ( 'NONE',  ( 12.11768468619488637, -5.101415283429129310, -15.63842114478006629 ) ) ;
#15372 = DIRECTION ( 'NONE',  ( -0.3542738219355896501, 0.000000000000000000, -0.9351417320872542627 ) ) ;
#15374 = ORIENTED_EDGE ( 'NONE', *, *, #8232, .T. ) ;
#15375 = ORIENTED_EDGE ( 'NONE', *, *, #12703, .T. ) ;
#15376 = CARTESIAN_POINT ( 'NONE',  ( 13.63565303003243478, 21.00494883119180045, 3.473673388005832585 ) ) ;
#15378 = DIRECTION ( 'NONE',  ( -0.9784543669157944601, 0.000000000000000000, -0.2064631973582987945 ) ) ;
#15377 = CARTESIAN_POINT ( 'NONE',  ( -0.1405913361260165972, 13.90873432424026213, 0.5585379980126942145 ) ) ;
#15379 = ORIENTED_EDGE ( 'NONE', *, *, #8817, .T. ) ;
#15380 = VERTEX_POINT ( 'NONE', #17954 ) ;
#15381 = PLANE ( 'NONE',  #21223 ) ;
#15382 = VERTEX_POINT ( 'NONE', #12885 ) ;
#15383 = CARTESIAN_POINT ( 'NONE',  ( 7.463375574167044668, 16.12223603717324849, -2.121406194095333930 ) ) ;
#15384 = AXIS2_PLACEMENT_3D ( 'NONE', #3102, #6301, #13075 ) ;
#15385 = LINE ( 'NONE', #4964, #17412 ) ;
#15386 = ORIENTED_EDGE ( 'NONE', *, *, #2047, .F. ) ;
#15387 = EDGE_CURVE ( 'NONE', #6924, #3547, #20992, .T. ) ;
#15388 = CARTESIAN_POINT ( 'NONE',  ( 27.40895291499714403, 32.54502000000000095, -9.088367920799473865 ) ) ;
#15389 = CARTESIAN_POINT ( 'NONE',  ( 60.38511073144201191, 0.000000000000000000, -22.26373525985038526 ) ) ;
#15390 = CARTESIAN_POINT ( 'NONE',  ( -0.1293393001420969635, 13.83032883076687725, 0.7266954706132912056 ) ) ;
#15391 = EDGE_CURVE ( 'NONE', #21133, #539, #9525, .T. ) ;
#15392 = DIRECTION ( 'NONE',  ( 0.000000000000000000, 1.000000000000000000, 0.000000000000000000 ) ) ;
#15393 = ORIENTED_EDGE ( 'NONE', *, *, #7000, .T. ) ;
#15394 = CARTESIAN_POINT ( 'NONE',  ( 5.013800915383680668, 12.10687735873178283, 5.308141424993535473 ) ) ;
#15395 = PLANE ( 'NONE',  #18072 ) ;
#15396 = FACE_OUTER_BOUND ( 'NONE', #18593, .T. ) ;
#15397 = FACE_OUTER_BOUND ( 'NONE', #14130, .T. ) ;
#15398 = AXIS2_PLACEMENT_3D ( 'NONE', #9329, #3842, #3734 ) ;
#15399 = DIRECTION ( 'NONE',  ( -0.6496772031432439531, 0.000000000000000000, 0.7602101891687401691 ) ) ;
#15400 = B_SPLINE_CURVE_WITH_KNOTS ( 'NONE', 3,
 ( #12416, #4222, #2115, #350, #3898, #5655, #10640, #4009, #10753, #17268, #10962, #15850, #14307, #21024, #2001, #5870, #17601, #3787, #7099, #9075, #2232, #13867, #2454, #5430, #9183, #12195, #17498, #7424, #10522, #470, #2342, #20912, #17392, #8856, #15639, #7223, #13984, #20681, #15963, #8971, #5774, #12530, #6302, #21122, #11077, #6416, #14635, #7646, #1327, #16491, #12861, #9512, #14845, #7752, #14407, #13186, #16388, #21560, #7859, #19783, #5971, #11179, #12744, #16177, #4448, #19466, #18148, #1225, #14738, #2890, #4657, #4337, #19581, #19895, #18033, #6091, #21444, #4768, #6198, #17715, #9622, #17932, #17832, #2679, #7968, #2566, #9300, #9408, #14514, #2777, #8069, #1003, #3003, #21340, #16281, #21234, #13076, #16075, #905, #1114, #12966, #19677, #4545, #11284, #11402, #9730, #14958, #20315, #3330, #8614, #8387, #18665, #16597, #4868, #16808, #15162, #19997, #1437, #3534, #6956, #6854, #18565, #11726, #15390, #10272, #18463, #13722, #3103, #20051, #17021, #10061, #11935, #11612, #21775, #18345, #13294, #13616, #20214, #8184, #3211, #1647, #5184, #8498, #9949, #1870, #9828, #11836, #21672, #5088, #3428, #217, #20418, #11501, #18244, #10163, #6534, #16710, #6739, #1548, #16906, #1755, #8291, #15063, #6626, #15280, #13392, #20100, #4970, #13503, #105, #2203, #18780, #10497, #15720, #10393, #20539, #2427, #14169, #15497, #20652, #7192, #15604, #18996, #12387, #3873, #761, #5625, #10825, #10610, #548, #324, #5746, #441, #2086, #7067, #12050, #20875, #3650, #12501, #7515, #17359, #15935, #3762, #7294, #8944, #13954, #12167, #17137, #18891, #9153, #13834, #19223, #4085, #2311, #5403, #7398, #1978, #19111, #8719, #20765, #14058, #17574, #14280, #5513, #3982, #5285, #17243, #8827, #12271, #10725, #17467, #9047, #15823, #650, #8045, #7829, #2981, #11375, #11047, #9705, #12833, #16255, #9267, #9593, #18004, #19756, #9378, #6061, #20997, #5844, #19651, #12601, #16146, #19554, #6176, #4421, #16471, #21315, #4628, #17902, #1085, #9484, #16362, #2862, #21202, #2536, #17801, #1201, #14607, #973, #2750, #14715, #12942, #7944, #16045, #4519, #7723, #14485, #876, #10932, #11257, #18122, #19325, #7619, #1303, #4192, #17683, #21421, #14378, #5944, #21094, #13049, #6275, #12710, #19434, #4308, #2649, #1524, #1625, #11910, #3307, #13159, #18325, #11697, #3185, #4945, #18435, #8155, #1845, #6718, #20290, #5159, #14818, #18639, #10138, #9807, #19871, #18542, #10039, #9917, #20078, #11813, #21531, #16787, #10246, #21859, #3507, #13271, #4849, #6827, #5061, #13588, #6391, #16576, #16991, #4746, #11483, #8268, #18227, #21648, #3084, #3405, #1412, #14934, #6511, #19978, #11589, #16683, #8366, #15039, #21753, #6607, #13371, #15139, #13473, #20189, #16883, #1733, #8473, #15249, #75, #17110, #13694, #931, #4365, #4254, #3735, #5378, #10365, #15364, #17749, #6931, #2595, #11103, #14229, #7571, #19501, #7035, #10881, #706, #17211, #10992, #17630, #20394, #294, #7455, #12558, #17857, #9330, #1950, #16101, #12020, #8690, #8587, #5802, #5258, #21153, #6008, #2054, #20945, #12778, #187, #19280, #13804, #2482, #15996, #14332, #20508, #12141, #8795, #18867, #4143, #5897, #12661, #10817, #1967, #5610, #20526, #20862, #7387, #9140, #7499, #19209, #5393, #3857, #12261, #20754, #17456, #10380, #310, #4076, #14157, #637, #2190, #17226, #15587, #12370, #5732, #12486, #10595, #13821, #15925, #8931, #19097, #12156, #17564, #9036, #2414, #2299, #748, #7053, #18984, #14265, #10711, #20639, #20982, #19317, #3966, #5834, #15811, #12592, #18881, #3752, #17127, #8705, #15484, #10485, #426, #17342, #2069, #8810, #7177, #14046, #15708, #13942, #5499, #536, #7284, #9693, #13147, #12697, #12930, #1294, #14594, #2848, #7606, #13036, #17891, #8033, #1073, #11360, #9254, #19421, #9473, #7816, #4295, #16033, #18110, #21517, #21410, #21189, #21083, #10922, #19741, #2525, #4615, #6374, #16243, #17992, #14809, #2637, #6165, #2737, #6047, #11035, #864, #17790, #4179, #9366, #2967, #16459, #17670, #16133, #14706, #14367, #962, #5933, #21302, #7712, #14473, #12818, #19544, #19639, #4409, #11143, #4507, #11244, #9580, #16350, #1188, #6265, #7930, #13359, #14918, #18314, #6598, #1396, #20278, #11473, #15129, #8138, #8460, #16875, #18630, #8255, #4934, #19860, #4733, #18531, #18217, #15028, #3070, #9796, #13574, #1722, #10130, #15232, #63, #3497, #21744, #11683, #16564, #21635, #3396, #6495, #20064, #18422, #5049, #3293, #15349, #20174, #10024, #4839, #3170, #8358, #6815, #5149, #16777, #13259, #16667, #11901, #21848, #1618, #6702, #10233, #13463, #16978, #19967, #11798, #1832, #8574, #9901, #177, #6919, #11574, #1510, #15455, #2388, #15898, #17540, #396, #3610, #20496, #1939, #5702, #2158, #17434, #19067, #7361, #13792, #7150, #8903, #9115, #5367, #12009, #17199, #10565, #2039, #3830, #17311, #7024, #724, #5582, #19185, #4051, #13682, #10795, #9014, #8681, #18740, #20726, #282, #20382, #616, #10350, #14131, #5249, #18958, #12341, #17094, #12129, #15683, #5472, #8784, #18853 ),
 .UNSPECIFIED., .F., .F.,
 ( 4, 3, 3, 3, 3, 3, 3, 3, 3, 3, 3, 3, 3, 3, 3, 3, 3, 3, 3, 3, 3, 3, 3, 3, 3, 3, 3, 3, 3, 3, 3, 3, 3, 3, 3, 3, 3, 3, 3, 3, 3, 3, 3, 3, 3, 3, 3, 3, 3, 3, 3, 3, 3, 3, 3, 3, 3, 3, 3, 3, 3, 3, 3, 3, 3, 3, 3, 3, 3, 3, 3, 3, 3, 3, 3, 3, 3, 3, 3, 3, 3, 3, 3, 3, 3, 3, 3, 3, 3, 3, 3, 3, 3, 3, 3, 3, 3, 3, 3, 3, 3, 3, 3, 3, 3, 3, 3, 3, 3, 3, 3, 3, 3, 3, 3, 3, 3, 3, 3, 3, 3, 3, 3, 3, 3, 3, 3, 3, 3, 3, 3, 3, 3, 3, 3, 3, 3, 3, 3, 3, 3, 3, 3, 3, 3, 3, 3, 3, 3, 3, 3, 3, 3, 3, 3, 3, 3, 3, 3, 3, 3, 3, 3, 3, 3, 3, 3, 3, 3, 3, 3, 3, 3, 3, 3, 3, 3, 3, 3, 3, 3, 3, 3, 3, 3, 3, 3, 3, 3, 3, 3, 3, 3, 3, 3, 3, 3, 3, 3, 3, 3, 3, 3, 3, 3, 3, 3, 3, 3, 3, 3, 3, 3, 3, 3, 3, 3, 3, 4 ),
 ( 0.000000000000000000, 0.006329113921512709816, 0.01249999948583089930, 0.01265822784302339868, 0.01898734176453509975, 0.02531645568604689797, 0.02874999970365120158, 0.03164556960755859905, 0.03797468352907030359, 0.04430379745058199426, 0.04500000460022859916, 0.05063291137210369774, 0.05696202529361540229, 0.06124999099804120245, 0.06329113921512709295, 0.06962025313663890158, 0.07594936705815059919, 0.07750001213348130247, 0.08227848097966231067, 0.08860759490117400827, 0.09374999174283218939, 0.09493670882268570588, 0.1012658227441869951, 0.1075949366657489997, 0.1100000114765239956, 0.1139240505872110010, 0.1202531645087729917, 0.1262499984399119979, 0.1265822784302340076, 0.1329113923517959983, 0.1392405062732580134, 0.1425000018589560047, 0.1455696201948190049, 0.1518987341162809923, 0.1582278480378430108, 0.1587500029336659790, 0.1645569619593049981, 0.1708860758808660174, 0.1749999920308009937, 0.1772151898023280048, 0.1835443037238899955, 0.1898734176453510114, 0.1912500109487239863, 0.1962025315669130021, 0.2025316454883749895, 0.2074999907470810034, 0.2088607594099370079, 0.2151898733313979961, 0.2215189872529599868, 0.2237500124104200017, 0.2278481011744220019, 0.2341772150959829935, 0.2399999971172069868, 0.2405063290174449808, 0.2468354429390069993, 0.2531645568604689589, 0.2562500040988209826, 0.2594936707820300059, 0.2658227847034919655, 0.2721518986250540117, 0.2725000015136869735, 0.2784810125465150277, 0.2848101264680770184, 0.2887499934460570072, 0.2911392403895390335, 0.2974683543111009687, 0.3037974682325620401, 0.3050000094647010163, 0.3101265821541239753, 0.3164556960755859905, 0.3212499901042359940, 0.3227848099971469820, 0.3291139239186089971, 0.3354430378401709878, 0.3375000129078500333, 0.3417721517616330029, 0.3481012656831939944, 0.3537499956223240094, 0.3544303796046560096, 0.3607594935262180003, 0.3670886074476790162, 0.3700000062353510089, 0.3734177213692410069, 0.3797468352907030220, 0.3860759492122649572, 0.3862500004432609657, 0.3924050631337259731, 0.3987341770552880194, 0.4024999951885679939, 0.4050632909767500345, 0.4113924048983109705, 0.4177215188197730411, 0.4187500077716679869, 0.4240506327413349763, 0.4303797466627969914, 0.4349999898663099995, 0.4367088605843579829, 0.4430379745058199981, 0.4493670884273820443, 0.4512500129516539560, 0.4556962023488430047, 0.4620253162704049954, 0.4674999940843199697, 0.4683544301918670105, 0.4746835441134290012, 0.4810126580348899616, 0.4837500081779320116, 0.4873417719564519524, 0.4936708858779140230, 0.4999999997994749590, 0.5063291137210370607, 0.5126582276424990203, 0.5162499971872059890, 0.5189873415640610110, 0.5253164554855219714, 0.5316455694070840732, 0.5325000059764910532, 0.5379746833285459218, 0.5443037972501070243, 0.5487499900616280568, 0.5506329111715689839, 0.5569620250931309746, 0.5632911390145930453, 0.5650000125471910106, 0.5696202529361540368, 0.5759493668576159964, 0.5812499926263350325, 0.5822784807791780981, 0.5886075947006399467, 0.5949367086222009382, 0.5975000098441739516, 0.6012658225436630088, 0.6075949364652249995, 0.6137499991490910078, 0.6139240503866860710, 0.6202531643082479507, 0.6265822782297100213, 0.6299999993587850344, 0.6329113921512710128, 0.6392405060727330834, 0.6455696199942949631, 0.6462500041965290043, 0.6518987339157570338, 0.6582278478373180253, 0.6624999906948350059, 0.6645569617587799849, 0.6708860756803419756, 0.6772151896018030470, 0.6787500117227039942, 0.6835443035233650377, 0.6898734174448269973, 0.6949999913591019540, 0.6962025313663889881, 0.7025316452878499485, 0.7088607592094120502, 0.7112500111636119726, 0.7151898731308740098, 0.7215189870524348903, 0.7274999980929279797, 0.7278481009738969609, 0.7341772148954590627, 0.7405063288169210223, 0.7437500016122360336, 0.7468354427384820138, 0.7531645566599439734, 0.7594936705815059641, 0.7600000025531850056, 0.7658227845029670355, 0.7721518984245289152, 0.7762499917481929801, 0.7784810123459909859, 0.7848101262675529766, 0.7911392401890140480, 0.7925000105295659791, 0.7974683541105760387, 0.8037974680320379983, 0.8087499903763730735, 0.8101265819535989898, 0.8164556958750610605, 0.8227848097966229401, 0.8250000120812989168, 0.8291139237180850108, 0.8354430376396460023, 0.8412499967467070849, 0.8417721515611080729, 0.8481012654826700636, 0.8544303794041309130, 0.8575000038524419610, 0.8607594933256930148, 0.8670886072471549744, 0.8734177211687170761, 0.8737500011633969610, 0.8797468350901779255, 0.8860759490117400272, 0.8899999931828780353, 0.8924050629332019868, 0.8987341768547630894, 0.9050632907762249380, 0.9062500090409180142, 0.9113924046977870397, 0.9177215186192489993, 0.9224999897505299362, 0.9240506325408099908, 0.9303797464622719504, 0.9367088603838339411, 0.9387500125608460033, 0.9430379743052960118, 0.9493670882268570033, 0.9549999952374580436, 0.9556962021483190739, 0.9620253160698809536, 0.9683544299913420250, 0.9712500058838849926, 0.9746835439129040157, 0.9810126578343659753, 0.9873417717559279660, 0.9875000001065180610, 0.9936708856773890375, 0.9999999995989510282 ),
 .UNSPECIFIED. ) ;
#15401 = EDGE_LOOP ( 'NONE', ( #9234, #13962, #19099, #10355 ) ) ;
#15402 = CARTESIAN_POINT ( 'NONE',  ( 6.184730801054771021, 10.88474977364208129, 3.317143460567523405 ) ) ;
#15403 = DIRECTION ( 'NONE',  ( -0.9129422336036514540, 0.000000000000000000, 0.4080888115383414783 ) ) ;
#15404 = CARTESIAN_POINT ( 'NONE',  ( 13.29405768023306855, 17.16992202419550040, 7.114197972723578012 ) ) ;
#15405 = ORIENTED_EDGE ( 'NONE', *, *, #5180, .T. ) ;
#15406 = ORIENTED_EDGE ( 'NONE', *, *, #8171, .F. ) ;
#15407 = LINE ( 'NONE', #8960, #8123 ) ;
#15408 = CARTESIAN_POINT ( 'NONE',  ( 8.854315084285317994, 11.17507848100337142, 4.651611944549387090 ) ) ;
#15409 = CARTESIAN_POINT ( 'NONE',  ( 2.934619771450872605, 20.19932627889173915, 2.180100518733211867 ) ) ;
#15410 = CARTESIAN_POINT ( 'NONE',  ( 7.735533989518945219, 25.39269750000000059, -21.17236077523805449 ) ) ;
#15411 = CARTESIAN_POINT ( 'NONE',  ( 5.587488707699998614, 15.19155588846434668, -1.244131986940470558 ) ) ;
#15412 = DIRECTION ( 'NONE',  ( 0.2868778675745011220, 0.000000000000000000, 0.9579671649362033747 ) ) ;
#15413 = CARTESIAN_POINT ( 'NONE',  ( 9.129586632131145407, 19.91511611422710359, 6.193789383866233678 ) ) ;
#15414 = CARTESIAN_POINT ( 'NONE',  ( 4.163685238762522722, 21.32044071393296036, 5.231111188599066431 ) ) ;
#15415 = CARTESIAN_POINT ( 'NONE',  ( 11.82678039945931481, 34.52875999999999834, -12.74436900065013667 ) ) ;
#15416 = ADVANCED_FACE ( 'NONE', ( #8640 ), #10186, .F. ) ;
#15417 = CARTESIAN_POINT ( 'NONE',  ( 1.202411175319977765, -7.547927499999999235, -22.85209084599881635 ) ) ;
#15418 = CARTESIAN_POINT ( 'NONE',  ( 0.3827680527341568162, 18.57760016544011705, 1.316900888515376566 ) ) ;
#15419 = CARTESIAN_POINT ( 'NONE',  ( 30.02465935949302533, -6.754812500000002551, -2.324128137548288731 ) ) ;
#15420 = DIRECTION ( 'NONE',  ( -0.9966381950048638361, 0.000000000000000000, 0.08192867786951606168 ) ) ;
#15421 = CARTESIAN_POINT ( 'NONE',  ( 10.96829523475326695, -1.381748506594268733, -17.00159016424930414 ) ) ;
#15422 = DIRECTION ( 'NONE',  ( 0.000000000000000000, 1.000000000000000000, 0.000000000000000000 ) ) ;
#15423 = CARTESIAN_POINT ( 'NONE',  ( 9.157588821307307114, 21.85973784873793235, 1.865442930748904216 ) ) ;
#15424 = FACE_OUTER_BOUND ( 'NONE', #808, .T. ) ;
#15425 = ORIENTED_EDGE ( 'NONE', *, *, #14253, .T. ) ;
#15426 = CARTESIAN_POINT ( 'NONE',  ( 11.32358359230530631, 12.92367503848713106, -2.306284810701165089 ) ) ;
#15427 = DIRECTION ( 'NONE',  ( -0.9987059298363657467, 0.000000000000000000, -0.05085730733808445370 ) ) ;
#15429 = DIRECTION ( 'NONE',  ( 0.6702301885068628895, 0.000000000000000000, 0.7421532822901579785 ) ) ;
#15428 = CARTESIAN_POINT ( 'NONE',  ( 5.668831867569799066, 12.20187417505221994, 1.017780631167809258 ) ) ;
#15430 = EDGE_LOOP ( 'NONE', ( #5905, #20177, #15782, #20006, #858 ) ) ;
#15431 = DIRECTION ( 'NONE',  ( 1.000000000000000000, 0.000000000000000000, 0.000000000000000000 ) ) ;
#15432 = CARTESIAN_POINT ( 'NONE',  ( -0.4828750084152318434, 20.32260066232836238, 5.240161191498525106 ) ) ;
#15433 = CARTESIAN_POINT ( 'NONE',  ( 4.495706609612955873, 19.71336308942898441, 0.7933311248715388952 ) ) ;
#15434 = CARTESIAN_POINT ( 'NONE',  ( 6.095663563013475006, 11.06004392628846134, 2.889821626036587432 ) ) ;
#15435 = VERTEX_POINT ( 'NONE', #13748 ) ;
#15436 = CARTESIAN_POINT ( 'NONE',  ( 6.462165521336576290, 11.60753147827898069, 3.224331916540620124 ) ) ;
#15437 = CARTESIAN_POINT ( 'NONE',  ( 8.601357627048034971, 11.53726303284714128, 3.530950561658094067 ) ) ;
#15438 = CARTESIAN_POINT ( 'NONE',  ( 1.758281139847138741, 12.61021756743670252, 7.885184424230324396 ) ) ;
#15439 = CARTESIAN_POINT ( 'NONE',  ( 13.33955114723241842, 16.76849418036265149, 7.284517011081861781 ) ) ;
#15440 = EDGE_CURVE ( 'NONE', #21489, #10463, #16251, .T. ) ;
#15441 = CARTESIAN_POINT ( 'NONE',  ( 2.063750000000000195, 8.334374999999999645, 10.71562499999999929 ) ) ;
#15442 = CARTESIAN_POINT ( 'NONE',  ( 13.34198401680142076, 0.1820865615191624709, -16.27895105414784638 ) ) ;
#15443 = UNCERTAINTY_MEASURE_WITH_UNIT (LENGTH_MEASURE( 1.000000000000000082E-05 ), #4485, 'distance_accuracy_value', 'NONE');
#15444 = DIRECTION ( 'NONE',  ( 0.000000000000000000, -1.000000000000000000, -0.000000000000000000 ) ) ;
#15445 = AXIS2_PLACEMENT_3D ( 'NONE', #7841, #6186, #14288 ) ;
#15446 = ORIENTED_EDGE ( 'NONE', *, *, #16908, .F. ) ;
#15447 = CARTESIAN_POINT ( 'NONE',  ( 11.18447833514740886, 14.12277392074263638, 6.311446057064062032 ) ) ;
#15448 = CARTESIAN_POINT ( 'NONE',  ( 9.992878607143374836, 20.90214019755116226, -1.685752229938785041 ) ) ;
#15449 = ORIENTED_EDGE ( 'NONE', *, *, #10762, .T. ) ;
#15450 = CARTESIAN_POINT ( 'NONE',  ( 30.33489826846160398, 1.984375000000000000, -2.417033907079745525 ) ) ;
#15451 = DIRECTION ( 'NONE',  ( -0.6050250551579474667, -0.7753173868113220069, 0.1811839737371539194 ) ) ;
#15453 = LINE ( 'NONE', #2156, #16967 ) ;
#15452 = CARTESIAN_POINT ( 'NONE',  ( 5.257238202180718467, 13.88483174882859217, 8.323134035216043003 ) ) ;
#15454 = ORIENTED_EDGE ( 'NONE', *, *, #12161, .T. ) ;
#15455 = CARTESIAN_POINT ( 'NONE',  ( 7.503791424408063016, 16.45334519770218407, 8.390729612094148138 ) ) ;
#15456 = CYLINDRICAL_SURFACE ( 'NONE', #4520, 1.191259999999999986 ) ;
#15457 = EDGE_LOOP ( 'NONE', ( #10487, #15479, #70, #5370, #11477, #13599 ) ) ;
#15458 = EDGE_CURVE ( 'NONE', #7937, #11569, #8875, .T. ) ;
#15459 = CARTESIAN_POINT ( 'NONE',  ( 0.2299619499110654997, 13.12625805216814712, 2.319564647753492359 ) ) ;
#15460 = VECTOR ( 'NONE', #951, 1000.000000000000000 ) ;
#15461 = CARTESIAN_POINT ( 'NONE',  ( -17.46249999999999858, 0.000000000000000000, 0.000000000000000000 ) ) ;
#15462 = ORIENTED_EDGE ( 'NONE', *, *, #9973, .T. ) ;
#15463 = CARTESIAN_POINT ( 'NONE',  ( 1.882899281740455066, 15.00618873593124825, 0.2860482631481570115 ) ) ;
#15464 = ADVANCED_FACE ( 'NONE', ( #20567 ), #13413, .T. ) ;
#15465 = CARTESIAN_POINT ( 'NONE',  ( 3.740646147519985476, 14.76563347569464213, -0.3756423018599123198 ) ) ;
#15466 = EDGE_CURVE ( 'NONE', #1261, #7354, #2829, .T. ) ;
#15467 = EDGE_CURVE ( 'NONE', #1525, #14117, #10959, .T. ) ;
#15468 = CARTESIAN_POINT ( 'NONE',  ( 67.40134256979101224, 32.54502000000000095, -13.30734117861468135 ) ) ;
#15469 = FACE_OUTER_BOUND ( 'NONE', #18770, .T. ) ;
#15470 = LINE ( 'NONE', #13472, #6540 ) ;
#15471 = DIRECTION ( 'NONE',  ( -0.9790635044817342925, 0.000000000000000000, 0.2035550397114870846 ) ) ;
#15472 = VERTEX_POINT ( 'NONE', #9297 ) ;
#15473 = CARTESIAN_POINT ( 'NONE',  ( 49.28028498622276032, 0.000000000000000000, -25.68670502218146368 ) ) ;
#15474 = CYLINDRICAL_SURFACE ( 'NONE', #8198, 0.5080000000000010063 ) ;
#15475 = PLANE ( 'NONE',  #9959 ) ;
#15477 = CARTESIAN_POINT ( 'NONE',  ( 15.48598371012319497, -7.240509137277070906, -14.97045021982148683 ) ) ;
#15476 = DIRECTION ( 'NONE',  ( 0.6702301885068652210, 0.000000000000000000, 0.7421532822901560911 ) ) ;
#15478 = EDGE_LOOP ( 'NONE', ( #14070, #15010, #16135, #15128 ) ) ;
#15479 = ORIENTED_EDGE ( 'NONE', *, *, #7880, .F. ) ;
#15480 = CARTESIAN_POINT ( 'NONE',  ( 9.637099489725157397, 21.04886798522784375, 3.438002499022450031 ) ) ;
#15482 = CARTESIAN_POINT ( 'NONE',  ( 30.41963056417667488, 0.000000000000000000, -8.653862521447852174 ) ) ;
#15481 = CARTESIAN_POINT ( 'NONE',  ( 1.696055354432304707, 16.44733452758824654, -0.8045495263988319268 ) ) ;
#15483 = ORIENTED_EDGE ( 'NONE', *, *, #20741, .T. ) ;
#15484 = CARTESIAN_POINT ( 'NONE',  ( 4.586192111020174877, 11.08290593202983310, 3.814641854836081425 ) ) ;
#15485 = ORIENTED_EDGE ( 'NONE', *, *, #12135, .F. ) ;
#15486 = DIRECTION ( 'NONE',  ( 0.000000000000000000, 0.000000000000000000, -1.000000000000000000 ) ) ;
#15487 = ORIENTED_EDGE ( 'NONE', *, *, #16700, .T. ) ;
#15488 = EDGE_CURVE ( 'NONE', #3091, #13712, #12741, .T. ) ;
#15489 = CARTESIAN_POINT ( 'NONE',  ( 7.677408542654871049, 18.01687583117972835, -1.852128230417407595 ) ) ;
#15490 = CARTESIAN_POINT ( 'NONE',  ( 65.64431122251959039, 30.56064500000000095, -11.29787305743958115 ) ) ;
#15491 = ORIENTED_EDGE ( 'NONE', *, *, #1701, .T. ) ;
#15492 = EDGE_CURVE ( 'NONE', #4938, #17811, #19463, .T. ) ;
#15493 = VECTOR ( 'NONE', #6642, 1000.000000000000000 ) ;
#15494 = EDGE_CURVE ( 'NONE', #11521, #13358, #17390, .T. ) ;
#15495 = CARTESIAN_POINT ( 'NONE',  ( 53.84486179190094646, 0.000000000000000000, -6.412645463410259872 ) ) ;
#15496 = CARTESIAN_POINT ( 'NONE',  ( 34.38097451710952868, 0.000000000000000000, 0.2081255904771098786 ) ) ;
#15497 = CARTESIAN_POINT ( 'NONE',  ( 1.245798919419617956, 21.00536303059330123, 3.318209283441092339 ) ) ;
#15498 = ORIENTED_EDGE ( 'NONE', *, *, #11833, .T. ) ;
#15499 = CARTESIAN_POINT ( 'NONE',  ( 7.153480333052655737, 18.17742714445450858, 7.324180098355732582 ) ) ;
#15500 = DIRECTION ( 'NONE',  ( -0.5087559856598092844, 0.000000000000000000, -0.8609107660235849613 ) ) ;
#15501 = LINE ( 'NONE', #6744, #57 ) ;
#15502 = CARTESIAN_POINT ( 'NONE',  ( 49.79678389823170903, -1.983739999999999837, -28.13445659451038594 ) ) ;
#15503 = ORIENTED_EDGE ( 'NONE', *, *, #13563, .F. ) ;
#15504 = CARTESIAN_POINT ( 'NONE',  ( 9.152014112632087972, 16.62671289803297370, 8.096787993944319695 ) ) ;
#15505 = DIRECTION ( 'NONE',  ( -0.05085730733808459941, 0.000000000000000000, 0.9987059298363656357 ) ) ;
#15506 = CARTESIAN_POINT ( 'NONE',  ( 13.07020640692051217, 18.72802180134034344, 6.676514015753832076 ) ) ;
#15507 = ORIENTED_EDGE ( 'NONE', *, *, #3869, .T. ) ;
#15508 = ORIENTED_EDGE ( 'NONE', *, *, #13387, .T. ) ;
#15509 = CARTESIAN_POINT ( 'NONE',  ( 12.87588295628459001, 21.37236768246749108, 0.5100726682396032885 ) ) ;
#15510 = CARTESIAN_POINT ( 'NONE',  ( 9.407243984221324240, 17.02847102510445865, 7.946678039590906018 ) ) ;
#15511 = CARTESIAN_POINT ( 'NONE',  ( 1.334794203082131148, 20.33449649584820307, 3.512594067846317891 ) ) ;
#15512 = LINE ( 'NONE', #13857, #15493 ) ;
#15513 = ADVANCED_FACE ( 'NONE', ( #7321 ), #12414, .F. ) ;
#15514 = CARTESIAN_POINT ( 'NONE',  ( 6.250389098271795341, 19.57090748711431161, -0.1645743329559772594 ) ) ;
#15515 = ADVANCED_FACE ( 'NONE', ( #14842 ), #8182, .T. ) ;
#15516 = EDGE_CURVE ( 'NONE', #12344, #9848, #8607, .T. ) ;
#15517 = CARTESIAN_POINT ( 'NONE',  ( -15.27766260488554195, 34.52875999999999834, -26.04727837583638461 ) ) ;
#15518 = CARTESIAN_POINT ( 'NONE',  ( 13.27675186413636688, 21.88443657126030217, 0.3155811547653178395 ) ) ;
#15519 = DIRECTION ( 'NONE',  ( 0.8583349619704303546, 0.000000000000000000, -0.5130897514657839498 ) ) ;
#15520 = CARTESIAN_POINT ( 'NONE',  ( 4.249701460077716320, 11.26224364954182100, 1.967523915872277929 ) ) ;
#15521 = DIRECTION ( 'NONE',  ( -0.9579671649362034858, 0.000000000000000000, 0.2868778675745010109 ) ) ;
#15522 = AXIS2_PLACEMENT_3D ( 'NONE', #11264, #6611, #18011 ) ;
#15523 = CARTESIAN_POINT ( 'NONE',  ( 19.76187703821956987, 0.0006356308824410450246, -14.87669286379018807 ) ) ;
#15524 = CARTESIAN_POINT ( 'NONE',  ( 1.874547060697949075, 16.41909622821189885, -0.01419169111653226234 ) ) ;
#15525 = CARTESIAN_POINT ( 'NONE',  ( 59.90456643211351917, -1.983739999999999837, -2.926035437812116946 ) ) ;
#15526 = CARTESIAN_POINT ( 'NONE',  ( 39.62791084302666178, 32.54502000000000095, -24.65774797299118859 ) ) ;
#15527 = CARTESIAN_POINT ( 'NONE',  ( 16.70007911672089662, -8.387532456226729494, -15.92482817259669581 ) ) ;
#15528 = CARTESIAN_POINT ( 'NONE',  ( 42.35466991749225940, -1.983739999999999837, -17.94967221382040279 ) ) ;
#15529 = CYLINDRICAL_SURFACE ( 'NONE', #6448, 3.174999999999999822 ) ;
#15530 = CARTESIAN_POINT ( 'NONE',  ( 11.43714432798503466, 15.67669137045964156, 7.541779987268694363 ) ) ;
#15531 = AXIS2_PLACEMENT_3D ( 'NONE', #4988, #4785, #15078 ) ;
#15532 = CARTESIAN_POINT ( 'NONE',  ( 49.13030338002142372, 42.06303499999999929, -2.154981381712871791 ) ) ;
#15533 = CARTESIAN_POINT ( 'NONE',  ( 11.39716744546816862, 12.54995360374833702, -1.947677416576856890 ) ) ;
#15534 = CARTESIAN_POINT ( 'NONE',  ( 27.93207353965470574, 0.000000000000000000, -8.388685343514779902 ) ) ;
#15536 = CARTESIAN_POINT ( 'NONE',  ( 29.76562500000000000, 1.984375000000000000, -4.317999999999999616 ) ) ;
#15535 = CARTESIAN_POINT ( 'NONE',  ( 7.018469835957150238, 16.59395432398027381, 7.891820759634939009 ) ) ;
#15537 = EDGE_LOOP ( 'NONE', ( #15487, #19515, #12253, #9604, #21404, #6346, #1270, #13604, #4952, #19641, #5175, #14877, #19364, #1928, #17804, #549, #7004, #558, #5131, #14598, #16950, #12871, #19629, #8776, #15714, #21661, #2088, #18020 ) ) ;
#15538 = DIRECTION ( 'NONE',  ( -0.4987171968201975503, 0.000000000000000000, 0.8667647648559581031 ) ) ;
#15539 = EDGE_CURVE ( 'NONE', #19746, #7932, #19899, .T. ) ;
#15540 = CARTESIAN_POINT ( 'NONE',  ( 1.670997140563193373, 34.12394749999999988, -22.76294857149378714 ) ) ;
#15541 = PRODUCT_DEFINITION_SHAPE ( 'NONE', 'NONE',  #21890 ) ;
#15542 = VERTEX_POINT ( 'NONE', #16385 ) ;
#15543 = CARTESIAN_POINT ( 'NONE',  ( 14.08960504820682580, 20.59139265233172367, 3.838791682861076637 ) ) ;
#15544 = CARTESIAN_POINT ( 'NONE',  ( 4.465258710612409310, 19.89810213900386060, 6.216219807304937284 ) ) ;
#15545 = AXIS2_PLACEMENT_3D ( 'NONE', #20623, #3733, #3403 ) ;
#15546 = VECTOR ( 'NONE', #21554, 1000.000000000000000 ) ;
#15547 = CARTESIAN_POINT ( 'NONE',  ( 5.836838028218656049, 12.69913397707368219, 0.1851268596130520583 ) ) ;
#15548 = CARTESIAN_POINT ( 'NONE',  ( 6.713027782948464584, 11.25617621838232196, 2.282006732609870081 ) ) ;
#15549 = CARTESIAN_POINT ( 'NONE',  ( 7.410451725513929944, 18.37204556237463393, -2.651051064885699304 ) ) ;
#15550 = DIRECTION ( 'NONE',  ( 0.2840839455009870340, -0.1392238476126010371, 0.9486374608692910160 ) ) ;
#15551 = CARTESIAN_POINT ( 'NONE',  ( 12.83914629888907655, -0.3229198055095354736, -16.44254515780370696 ) ) ;
#15552 = CYLINDRICAL_SURFACE ( 'NONE', #8116, 0.7950200000000010592 ) ;
#15553 = VECTOR ( 'NONE', #14559, 1000.000000000000227 ) ;
#15554 = SHAPE_REPRESENTATION ( 'MAS-676', ( #21465, #9105, #6297, #2773, #16548, #3482, #13725, #6995, #19709 ), #8404 ) ;
#15555 = EDGE_LOOP ( 'NONE', ( #16013, #20728, #19622, #5783, #17234, #8284, #9166, #15696, #16110, #18307, #11493, #5706 ) ) ;
#15556 = CARTESIAN_POINT ( 'NONE',  ( 9.801219140300959864, 21.83972979323944230, 3.592275403358046404 ) ) ;
#15557 = ORIENTED_EDGE ( 'NONE', *, *, #13561, .T. ) ;
#15558 = CARTESIAN_POINT ( 'NONE',  ( 9.878043619689368171, 11.67119934733697129, 0.3244805056039586910 ) ) ;
#15559 = FACE_OUTER_BOUND ( 'NONE', #20773, .T. ) ;
#15560 = LINE ( 'NONE', #14125, #8904 ) ;
#15562 = CYLINDRICAL_SURFACE ( 'NONE', #18726, 1.587500000000002132 ) ;
#15561 = CARTESIAN_POINT ( 'NONE',  ( 1.566802806665559045, 21.20295136681662385, 5.074033647315427054 ) ) ;
#15563 = ORIENTED_EDGE ( 'NONE', *, *, #20540, .T. ) ;
#15564 = EDGE_CURVE ( 'NONE', #15989, #15924, #17929, .T. ) ;
#15565 = ORIENTED_EDGE ( 'NONE', *, *, #19385, .T. ) ;
#15566 = B_SPLINE_CURVE_WITH_KNOTS ( 'NONE', 3,
 ( #6421, #19681, #14744, #21450, #11407, #7199, #110, #20220, #11841, #11941, #13839, #13508 ),
 .UNSPECIFIED., .F., .F.,
 ( 4, 2, 2, 2, 2, 4 ),
 ( 0.003179145944081267997, 0.003422139863241870604, 0.003665133782402473211, 0.004151121620723678858, 0.004637109459044884072, 0.005123097297366089285 ),
 .UNSPECIFIED. ) ;
#15567 = STYLED_ITEM ( 'NONE', ( #16508 ), #6635 ) ;
#15568 = CARTESIAN_POINT ( 'NONE',  ( 52.19198938901277529, 0.000000000000000000, 3.449560060533523487 ) ) ;
#15569 = VERTEX_POINT ( 'NONE', #14632 ) ;
#15570 = CIRCLE ( 'NONE', #687, 0.5079999999999976756 ) ;
#15571 = DIRECTION ( 'NONE',  ( -0.6702301885068630005, 0.000000000000000000, -0.7421532822901579785 ) ) ;
#15572 = CARTESIAN_POINT ( 'NONE',  ( 43.49132289107146931, 32.54502000000000095, 4.686923926377883021 ) ) ;
#15573 = DIRECTION ( 'NONE',  ( -0.2868778675745008999, 0.000000000000000000, -0.9579671649362034858 ) ) ;
#15574 = DIRECTION ( 'NONE',  ( 0.9685006480810790519, 0.000000000000000000, 0.2490110332224857170 ) ) ;
#15575 = EDGE_LOOP ( 'NONE', ( #1938, #17201, #19734, #18183 ) ) ;
#15576 = DIRECTION ( 'NONE',  ( -0.3482992169606098365, 0.9330960544336215357, -0.08955115110948595747 ) ) ;
#15577 = LINE ( 'NONE', #526, #18424 ) ;
#15579 = CARTESIAN_POINT ( 'NONE',  ( 17.21645753443902649, -6.938450633991601002, -14.61028308222959637 ) ) ;
#15578 = LINE ( 'NONE', #17117, #11275 ) ;
#15580 = ORIENTED_EDGE ( 'NONE', *, *, #3589, .F. ) ;
#15581 = ORIENTED_EDGE ( 'NONE', *, *, #12494, .F. ) ;
#15582 = CARTESIAN_POINT ( 'NONE',  ( 6.497796024369758783, 11.60753147827898069, 3.213661819375602136 ) ) ;
#15583 = CIRCLE ( 'NONE', #10975, 3.174999999999998490 ) ;
#15585 = PLANE ( 'NONE',  #6426 ) ;
#15584 = CARTESIAN_POINT ( 'NONE',  ( 2.908793012413193324, 11.23804227924006227, 5.217805794380214301 ) ) ;
#15586 = ORIENTED_EDGE ( 'NONE', *, *, #17802, .F. ) ;
#15588 = CARTESIAN_POINT ( 'NONE',  ( 10.65449937457216656, -4.912466459170417465, -16.01747763323893281 ) ) ;
#15587 = CARTESIAN_POINT ( 'NONE',  ( 5.530698010192272918, 13.68895168523844674, 8.102282649766468836 ) ) ;
#15589 = ORIENTED_EDGE ( 'NONE', *, *, #1404, .F. ) ;
#15590 = EDGE_CURVE ( 'NONE', #2743, #7573, #12159, .T. ) ;
#15591 = ORIENTED_EDGE ( 'NONE', *, *, #1644, .F. ) ;
#15592 = EDGE_CURVE ( 'NONE', #15542, #1856, #4394, .T. ) ;
#15593 = AXIS2_PLACEMENT_3D ( 'NONE', #7551, #20919, #12303 ) ;
#15594 = CARTESIAN_POINT ( 'NONE',  ( 7.470178629798640557, 16.24275013615479679, -2.126460335357540199 ) ) ;
#15595 = EDGE_LOOP ( 'NONE', ( #20500, #2268, #19422, #10921 ) ) ;
#15596 = CARTESIAN_POINT ( 'NONE',  ( 3.326019219354948486, 13.57811087000449035, 7.466394700117205296 ) ) ;
#15597 = CIRCLE ( 'NONE', #3570, 0.7950200000000003930 ) ;
#15598 = VECTOR ( 'NONE', #942, 1000.000000000000000 ) ;
#15599 = AXIS2_PLACEMENT_3D ( 'NONE', #7470, #17642, #14344 ) ;
#15600 = DIRECTION ( 'NONE',  ( 0.9964481331860213231, 0.000000000000000000, -0.08420877549337293932 ) ) ;
#15601 = LINE ( 'NONE', #19108, #4388 ) ;
#15602 = LINE ( 'NONE', #2309, #503 ) ;
#15603 = DIRECTION ( 'NONE',  ( -0.2672484743474505819, 0.000000000000000000, -0.9636276526537416176 ) ) ;
#15604 = CARTESIAN_POINT ( 'NONE',  ( 1.327372290668605848, 21.07154981679812167, 3.536567113229659665 ) ) ;
#15605 = FACE_OUTER_BOUND ( 'NONE', #12029, .T. ) ;
#15606 = VERTEX_POINT ( 'NONE', #6954 ) ;
#15607 = CARTESIAN_POINT ( 'NONE',  ( 4.101782029537222485, 17.20635281421107265, -0.8596899216323250492 ) ) ;
#15608 = DIRECTION ( 'NONE',  ( -0.3542738219355896501, 0.000000000000000000, -0.9351417320872542627 ) ) ;
#15609 = DIRECTION ( 'NONE',  ( 0.8609107660235850723, 0.000000000000000000, -0.5087559856598092844 ) ) ;
#15610 = CARTESIAN_POINT ( 'NONE',  ( 23.49608546833631451, 3.565842500000000914, -17.12016812500874252 ) ) ;
#15611 = EDGE_CURVE ( 'NONE', #15199, #10916, #13501, .T. ) ;
#15612 = CIRCLE ( 'NONE', #11713, 30.16250000000000497 ) ;
#15613 = ORIENTED_EDGE ( 'NONE', *, *, #9918, .F. ) ;
#15614 = CARTESIAN_POINT ( 'NONE',  ( 8.856615887970798795, 13.10471967957858119, 6.770334555984388381 ) ) ;
#15615 = CYLINDRICAL_SURFACE ( 'NONE', #20167, 0.7950200000000000600 ) ;
#15616 = B_SPLINE_CURVE_WITH_KNOTS ( 'NONE', 3,
 ( #7536, #3672, #15743, #4108, #17386 ),
 .UNSPECIFIED., .F., .F.,
 ( 4, 1, 4 ),
 ( 0.003699823995550772550, 0.003727086906962205105, 0.003754349818373638095 ),
 .UNSPECIFIED. ) ;
#15617 = CARTESIAN_POINT ( 'NONE',  ( 11.32059934594350281, 22.04125121511821916, 2.023640860796339869 ) ) ;
#15618 = EDGE_LOOP ( 'NONE', ( #4984, #11234, #21011, #15110 ) ) ;
#15619 = CIRCLE ( 'NONE', #2883, 2.182812499999997158 ) ;
#15620 = ORIENTED_EDGE ( 'NONE', *, *, #17775, .T. ) ;
#15621 = CARTESIAN_POINT ( 'NONE',  ( -15.60052840353961656, -2.331258458467470263, -10.41609846181393451 ) ) ;
#15622 = CIRCLE ( 'NONE', #16662, 1.587500000000001688 ) ;
#15623 = VECTOR ( 'NONE', #18901, 1000.000000000000000 ) ;
#15624 = CARTESIAN_POINT ( 'NONE',  ( 9.139755265305351983, 11.93170736937736187, 5.902681470851192103 ) ) ;
#15625 = CARTESIAN_POINT ( 'NONE',  ( -0.7765736244451648673, 19.84689652320655995, 3.563773667300057291 ) ) ;
#15626 = DIRECTION ( 'NONE',  ( -0.9685006480810792739, 0.000000000000000000, -0.2490110332224850509 ) ) ;
#15627 = ADVANCED_FACE ( 'NONE', ( #3328 ), #3426, .F. ) ;
#15628 = CARTESIAN_POINT ( 'NONE',  ( 5.995600430637586520, 12.23416120028617371, 1.046533783840128740 ) ) ;
#15629 = CARTESIAN_POINT ( 'NONE',  ( 7.142136784733786214, 17.57921760804553557, 7.468824909625386255 ) ) ;
#15630 = CIRCLE ( 'NONE', #5728, 0.7950200000000003930 ) ;
#15631 = CIRCLE ( 'NONE', #9249, 19.05000000000000071 ) ;
#15632 = CARTESIAN_POINT ( 'NONE',  ( 1.396705373849880472, 20.30655539761074735, 3.754731929609379737 ) ) ;
#15633 = CARTESIAN_POINT ( 'NONE',  ( 46.03750000000000142, 34.52875999999999834, -10.31874999999999964 ) ) ;
#15634 = EDGE_CURVE ( 'NONE', #7573, #15261, #3648, .T. ) ;
#15635 = CARTESIAN_POINT ( 'NONE',  ( 11.23574321677510213, 19.52774875955264022, 6.574244702891200554 ) ) ;
#15636 = CARTESIAN_POINT ( 'NONE',  ( 4.867729296808080974, 12.11136722865829540, 5.091807635075894289 ) ) ;
#15637 = AXIS2_PLACEMENT_3D ( 'NONE', #8470, #5058, #20287 ) ;
#15638 = CARTESIAN_POINT ( 'NONE',  ( 3.690010452587021206, 17.35406872798134259, -1.479586497304065329 ) ) ;
#15639 = CARTESIAN_POINT ( 'NONE',  ( 1.431034899629216817, 18.16898401507852867, 9.266644725746632005 ) ) ;
#15640 = AXIS2_PLACEMENT_3D ( 'NONE', #13053, #19656, #6180 ) ;
#15641 = CARTESIAN_POINT ( 'NONE',  ( 19.76338907927813437, -0.001881842415276016372, -14.87633619820457653 ) ) ;
#15642 = CARTESIAN_POINT ( 'NONE',  ( 3.122877388456776426, 12.59229297301672190, 6.489217028501734319 ) ) ;
#15643 = DIRECTION ( 'NONE',  ( 0.000000000000000000, 1.000000000000000000, 0.000000000000000000 ) ) ;
#15644 = FACE_BOUND ( 'NONE', #6152, .T. ) ;
#15645 = CARTESIAN_POINT ( 'NONE',  ( 18.02971726292177124, 1.782683163403355309, -14.85524908451608006 ) ) ;
#15646 = EDGE_CURVE ( 'NONE', #19832, #10888, #20313, .T. ) ;
#15647 = ADVANCED_FACE ( 'NONE', ( #11933 ), #3532, .T. ) ;
#15648 = FACE_OUTER_BOUND ( 'NONE', #6772, .T. ) ;
#15649 = VECTOR ( 'NONE', #3258, 1000.000000000000227 ) ;
#15650 = EDGE_CURVE ( 'NONE', #8830, #17565, #6149, .T. ) ;
#15651 = DIRECTION ( 'NONE',  ( -0.2490110332224850509, 0.000000000000000000, 0.9685006480810792739 ) ) ;
#15652 = CARTESIAN_POINT ( 'NONE',  ( 11.28297949870794170, 17.68526700538642515, 7.421515332377799368 ) ) ;
#15653 = DIRECTION ( 'NONE',  ( 0.000000000000000000, 1.000000000000000000, 0.000000000000000000 ) ) ;
#15654 = CARTESIAN_POINT ( 'NONE',  ( 12.11045644880566741, 11.20221354020535109, 1.207418464437750805 ) ) ;
#15655 = LINE ( 'NONE', #10535, #12683 ) ;
#15656 = ORIENTED_EDGE ( 'NONE', *, *, #8002, .F. ) ;
#15657 = DIRECTION ( 'NONE',  ( -0.2672484743474491942, 0.000000000000000000, -0.9636276526537419507 ) ) ;
#15658 = AXIS2_PLACEMENT_3D ( 'NONE', #6605, #15246, #11809 ) ;
#15659 = CARTESIAN_POINT ( 'NONE',  ( -6.268352501591477832, -0.7997824999999986195, -35.49402737582407497 ) ) ;
#15660 = CIRCLE ( 'NONE', #8915, 0.3962400000000012579 ) ;
#15661 = CARTESIAN_POINT ( 'NONE',  ( 11.66121486338230895, -6.991816407965024460, -15.94738478811983562 ) ) ;
#15662 = VERTEX_POINT ( 'NONE', #7190 ) ;
#15663 = CIRCLE ( 'NONE', #1520, 4.961572499999999941 ) ;
#15664 = CARTESIAN_POINT ( 'NONE',  ( 9.355592019679061622, 15.41930233576164433, -2.894346530100807335 ) ) ;
#15665 = CARTESIAN_POINT ( 'NONE',  ( 10.33042288919505580, 11.26312240063166037, 2.170817215344111872 ) ) ;
#15666 = CARTESIAN_POINT ( 'NONE',  ( 0.9885671785712810689, 20.25378384025834322, 1.764069577497025421 ) ) ;
#15667 = CARTESIAN_POINT ( 'NONE',  ( -22.47451353405102026, -10.87373999999999974, -25.43908013252627853 ) ) ;
#15668 = DIRECTION ( 'NONE',  ( 0.000000000000000000, 1.000000000000000000, 0.000000000000000000 ) ) ;
#15669 = CIRCLE ( 'NONE', #18460, 0.7950199999999982836 ) ;
#15670 = CARTESIAN_POINT ( 'NONE',  ( 19.49661015955114607, -1.441193557778313483, -14.33538266661406979 ) ) ;
#15671 = EDGE_CURVE ( 'NONE', #12065, #18576, #1713, .T. ) ;
#15672 = CARTESIAN_POINT ( 'NONE',  ( 42.66304184606194383, -9.531985000000000596, -19.22597499813143784 ) ) ;
#15673 = EDGE_LOOP ( 'NONE', ( #2609, #16661, #3199, #4508 ) ) ;
#15674 = CARTESIAN_POINT ( 'NONE',  ( 8.230913307447869087, 21.33050868956278023, 5.055680035315745613 ) ) ;
#15675 = EDGE_LOOP ( 'NONE', ( #10261, #8514 ) ) ;
#15676 = CARTESIAN_POINT ( 'NONE',  ( 10.15327187727333857, 11.38490435674824219, 1.527704889486475759 ) ) ;
#15677 = DIRECTION ( 'NONE',  ( 0.000000000000000000, 0.000000000000000000, 1.000000000000000000 ) ) ;
#15678 = AXIS2_PLACEMENT_3D ( 'NONE', #672, #9069, #14192 ) ;
#15679 = CARTESIAN_POINT ( 'NONE',  ( -22.90596259062238005, -8.889364999999999739, -9.869321627248080375 ) ) ;
#15681 = CYLINDRICAL_SURFACE ( 'NONE', #5685, 2.381250000000001421 ) ;
#15680 = CARTESIAN_POINT ( 'NONE',  ( 1.273922206673044455, 17.31795573271877942, 9.619519439844173903 ) ) ;
#15682 = ORIENTED_EDGE ( 'NONE', *, *, #7042, .T. ) ;
#15683 = CARTESIAN_POINT ( 'NONE',  ( 6.552291428502512893, 10.92726696357779126, 3.523081400066527369 ) ) ;
#15684 = DIRECTION ( 'NONE',  ( 0.000000000000000000, -1.000000000000000000, -0.000000000000000000 ) ) ;
#15685 = ORIENTED_EDGE ( 'NONE', *, *, #1657, .T. ) ;
#15686 = CYLINDRICAL_SURFACE ( 'NONE', #13232, 0.3962400000000010358 ) ;
#15687 = AXIS2_PLACEMENT_3D ( 'NONE', #1142, #1249, #6221 ) ;
#15688 = CARTESIAN_POINT ( 'NONE',  ( 11.74480790566189015, -4.503994935255103194, -15.66770688877914353 ) ) ;
#15689 = ORIENTED_EDGE ( 'NONE', *, *, #20065, .T. ) ;
#15690 = FACE_OUTER_BOUND ( 'NONE', #10944, .T. ) ;
#15691 = VECTOR ( 'NONE', #7155, 1000.000000000000000 ) ;
#15692 = LINE ( 'NONE', #14141, #13889 ) ;
#15693 = DIRECTION ( 'NONE',  ( 0.000000000000000000, 1.000000000000000000, 0.000000000000000000 ) ) ;
#15694 = EDGE_CURVE ( 'NONE', #3737, #877, #5795, .T. ) ;
#15695 = DIRECTION ( 'NONE',  ( 0.000000000000000000, -1.000000000000000000, 0.000000000000000000 ) ) ;
#15696 = ORIENTED_EDGE ( 'NONE', *, *, #13997, .F. ) ;
#15697 = DIRECTION ( 'NONE',  ( 0.3447671952293626108, 0.000000000000000000, 0.9386882235831439658 ) ) ;
#15698 = PLANE ( 'NONE',  #20899 ) ;
#15699 = DIRECTION ( 'NONE',  ( -0.9685006480810794960, 0.000000000000000000, -0.2490110332224836354 ) ) ;
#15701 = CARTESIAN_POINT ( 'NONE',  ( 19.75795317206712198, -3.625818983740633605, -14.16333780485109273 ) ) ;
#15700 = DIRECTION ( 'NONE',  ( 0.000000000000000000, -1.000000000000000000, -0.000000000000000000 ) ) ;
#15702 = ORIENTED_EDGE ( 'NONE', *, *, #2901, .F. ) ;
#15703 = ORIENTED_EDGE ( 'NONE', *, *, #9544, .T. ) ;
#15704 = CARTESIAN_POINT ( 'NONE',  ( 6.845745190715632589, 12.02592060257602213, 4.770099056714289354 ) ) ;
#15706 = DIRECTION ( 'NONE',  ( -0.000000000000000000, 1.000000000000000000, 0.000000000000000000 ) ) ;
#15705 = CARTESIAN_POINT ( 'NONE',  ( 3.428347309981619517, 18.28257875309041935, 8.925423822362398951 ) ) ;
#15707 = ORIENTED_EDGE ( 'NONE', *, *, #11055, .T. ) ;
#15709 = CARTESIAN_POINT ( 'NONE',  ( 19.84261803441996719, 0.4717451776687191511, -13.82102401822954718 ) ) ;
#15708 = CARTESIAN_POINT ( 'NONE',  ( 4.218746967243003354, 11.29694704288618290, 2.241506840608003870 ) ) ;
#15710 = ORIENTED_EDGE ( 'NONE', *, *, #16168, .F. ) ;
#15711 = ORIENTED_EDGE ( 'NONE', *, *, #16039, .F. ) ;
#15712 = AXIS2_PLACEMENT_3D ( 'NONE', #215, #10161, #16904 ) ;
#15713 = CARTESIAN_POINT ( 'NONE',  ( 7.596779357869561267, 13.14120497759026307, -0.9199170277768317083 ) ) ;
#15714 = ORIENTED_EDGE ( 'NONE', *, *, #12213, .T. ) ;
#15715 = CIRCLE ( 'NONE', #20258, 0.5079999999999996740 ) ;
#15716 = CARTESIAN_POINT ( 'NONE',  ( 14.35012762246612006, 0.3010510652611559923, 9.783890749713020085 ) ) ;
#15717 = DIRECTION ( 'NONE',  ( 0.7421532822901572013, 0.000000000000000000, -0.6702301885068637777 ) ) ;
#15718 = CARTESIAN_POINT ( 'NONE',  ( 1.782353389576713409, 23.59070174808080012, 8.727807302940615131 ) ) ;
#15719 = FACE_OUTER_BOUND ( 'NONE', #19059, .T. ) ;
#15720 = CARTESIAN_POINT ( 'NONE',  ( 0.9406339474007729962, 20.66888917947650484, 2.506880476070809660 ) ) ;
#15721 = EDGE_CURVE ( 'NONE', #12131, #10480, #3980, .T. ) ;
#15722 = DIRECTION ( 'NONE',  ( 1.000000000000000000, 0.000000000000000000, 0.000000000000000000 ) ) ;
#15723 = ORIENTED_EDGE ( 'NONE', *, *, #12819, .F. ) ;
#15724 = CARTESIAN_POINT ( 'NONE',  ( 0.7338959141973584455, 18.79999059560985231, 0.8591482719905695342 ) ) ;
#15725 = AXIS2_PLACEMENT_3D ( 'NONE', #12989, #7666, #2695 ) ;
#15726 = CARTESIAN_POINT ( 'NONE',  ( -1.351150467732365579, 2.373947500000000765, -27.17319717629097653 ) ) ;
#15727 = CARTESIAN_POINT ( 'NONE',  ( 29.64606458365116737, -1.985327499999998357, -15.53894806404596096 ) ) ;
#15728 = CARTESIAN_POINT ( 'NONE',  ( 28.87608719841374949, -7.547927499999999235, -15.73691681567849976 ) ) ;
#15729 = ORIENTED_EDGE ( 'NONE', *, *, #17622, .F. ) ;
#15730 = ORIENTED_EDGE ( 'NONE', *, *, #17924, .T. ) ;
#15731 = CARTESIAN_POINT ( 'NONE',  ( 5.026532476923114778, 15.50533030672313828, -1.679517137562626772 ) ) ;
#15732 = CYLINDRICAL_SURFACE ( 'NONE', #14206, 1.785937500000001510 ) ;
#15733 = CARTESIAN_POINT ( 'NONE',  ( 13.22358791529405408, 12.74046206659965819, 5.993796513000479997 ) ) ;
#15734 = ORIENTED_EDGE ( 'NONE', *, *, #21383, .T. ) ;
#15735 = AXIS2_PLACEMENT_3D ( 'NONE', #12049, #13615, #5183 ) ;
#15736 = ORIENTED_EDGE ( 'NONE', *, *, #19522, .T. ) ;
#15737 = CARTESIAN_POINT ( 'NONE',  ( 71.03963378001139972, 32.54502000000000095, -10.54138470677948014 ) ) ;
#15738 = CARTESIAN_POINT ( 'NONE',  ( 7.410350071410004347, 12.70579758959303796, -1.564945618823073925 ) ) ;
#15739 = CARTESIAN_POINT ( 'NONE',  ( 7.091083114709308965, 18.17949408554134649, 7.347600680106210369 ) ) ;
#15740 = CARTESIAN_POINT ( 'NONE',  ( 31.75000000000000000, 32.54502000000000095, -4.317999999999999616 ) ) ;
#15741 = CARTESIAN_POINT ( 'NONE',  ( 5.725034261819131665, 13.29448173139118161, -0.2693480136903509403 ) ) ;
#15742 = CARTESIAN_POINT ( 'NONE',  ( 7.319589578518462147, 14.78174204738065356, 7.369222843865381734 ) ) ;
#15743 = CARTESIAN_POINT ( 'NONE',  ( 38.98665935137078975, 37.69761546401537089, -3.914726640478982667 ) ) ;
#15744 = ADVANCED_FACE ( 'NONE', ( #5401 ), #17465, .T. ) ;
#15745 = CARTESIAN_POINT ( 'NONE',  ( 11.45406335465086833, 12.08730048838598314, 5.725135792998135464 ) ) ;
#15746 = AXIS2_PLACEMENT_3D ( 'NONE', #20077, #4944, #11696 ) ;
#15747 = DIRECTION ( 'NONE',  ( 0.9579671649362032637, 1.243294375783199532E-16, -0.2868778675745010664 ) ) ;
#15748 = CARTESIAN_POINT ( 'NONE',  ( 2.448534668620959476, 11.21351766718956178, 3.448322903900380432 ) ) ;
#15749 = CARTESIAN_POINT ( 'NONE',  ( 11.82678039945931481, -3.968114999999999615, -12.74436900065013667 ) ) ;
#15750 = EDGE_CURVE ( 'NONE', #4584, #304, #15602, .T. ) ;
#15751 = EDGE_CURVE ( 'NONE', #10775, #9189, #1893, .T. ) ;
#15752 = CARTESIAN_POINT ( 'NONE',  ( -12.30312499999999964, 1.984375000000000000, -2.268784209304649746 ) ) ;
#15753 = CARTESIAN_POINT ( 'NONE',  ( -0.3242065045807352996, 20.30684170721071879, 4.841807950102050562 ) ) ;
#15754 = DIRECTION ( 'NONE',  ( -0.1065921516619563053, -0.9937903127262235348, 0.03192064434796804129 ) ) ;
#15755 = DIRECTION ( 'NONE',  ( -0.3482992169606098365, 0.9330960544336215357, -0.08955115110948595747 ) ) ;
#15756 = CARTESIAN_POINT ( 'NONE',  ( 20.91780793311170328, -3.648416207543188960, -13.87012058890019972 ) ) ;
#15757 = FACE_OUTER_BOUND ( 'NONE', #4754, .T. ) ;
#15758 = CARTESIAN_POINT ( 'NONE',  ( 10.31539917732810707, 10.57772775276799315, 2.222527011904729122 ) ) ;
#15759 = ORIENTED_EDGE ( 'NONE', *, *, #12450, .F. ) ;
#15760 = DIRECTION ( 'NONE',  ( -0.9943660382494290406, 0.000000000000000000, 0.1060008583745199739 ) ) ;
#15761 = CARTESIAN_POINT ( 'NONE',  ( 11.21902111245313627, 16.87095629309551725, -3.573519051852731554 ) ) ;
#15762 = CARTESIAN_POINT ( 'NONE',  ( 16.97011862608863098, 1.212343544023858355, -15.21366445222733077 ) ) ;
#15763 = CARTESIAN_POINT ( 'NONE',  ( 0.04635182712760341911, 17.19594618500607908, 0.8198292707330264717 ) ) ;
#15764 = EDGE_LOOP ( 'NONE', ( #11271, #11814, #16712, #5330 ) ) ;
#15765 = SHAPE_DEFINITION_REPRESENTATION ( #21496, #560 ) ;
#15766 = VECTOR ( 'NONE', #16100, 1000.000000000000000 ) ;
#15767 = CARTESIAN_POINT ( 'NONE',  ( -0.08564316121918838509, 21.03045532789668925, 5.121204207707737766 ) ) ;
#15768 = FACE_BOUND ( 'NONE', #9132, .T. ) ;
#15769 = EDGE_CURVE ( 'NONE', #1966, #16810, #11152, .T. ) ;
#15770 = CARTESIAN_POINT ( 'NONE',  ( 20.34298345951636122, -6.628736041427409909, -15.10255183750635766 ) ) ;
#15771 = ORIENTED_EDGE ( 'NONE', *, *, #4165, .F. ) ;
#15772 = CARTESIAN_POINT ( 'NONE',  ( 6.062168776474054610, 18.80106227311165767, -0.8723543407741434219 ) ) ;
#15773 = CARTESIAN_POINT ( 'NONE',  ( 8.224353621346322640, 11.48768387232824217, 1.845154662582578542 ) ) ;
#15774 = CARTESIAN_POINT ( 'NONE',  ( 3.175397852148950761, 11.32322398379630179, 5.121166436712352166 ) ) ;
#15775 = CARTESIAN_POINT ( 'NONE',  ( 22.05855709630448303, 3.961447500000001565, -44.85793026951184004 ) ) ;
#15776 = EDGE_CURVE ( 'NONE', #11237, #10813, #19649, .T. ) ;
#15777 = CARTESIAN_POINT ( 'NONE',  ( 39.62791084302666178, 34.52875999999999834, -24.65774797299118859 ) ) ;
#15778 = CARTESIAN_POINT ( 'NONE',  ( 17.58887540853269371, 0.6711474593645572195, -14.96568140522104606 ) ) ;
#15779 = DIRECTION ( 'NONE',  ( -0.9959941601142527912, 0.000000000000000000, -0.08941830359777887260 ) ) ;
#15780 = ORIENTED_EDGE ( 'NONE', *, *, #16728, .T. ) ;
#15781 = CARTESIAN_POINT ( 'NONE',  ( 11.33455399463139734, 17.71700346048863395, 7.528911907053374541 ) ) ;
#15782 = ORIENTED_EDGE ( 'NONE', *, *, #6111, .T. ) ;
#15783 = CARTESIAN_POINT ( 'NONE',  ( 10.64372375218282407, 11.67083583707339045, 3.665092760906087044 ) ) ;
#15784 = DIRECTION ( 'NONE',  ( -0.000000000000000000, 1.000000000000000000, 0.000000000000000000 ) ) ;
#15785 = CARTESIAN_POINT ( 'NONE',  ( 13.21690244079663934, 22.21723637171626464, 1.444646363038201597 ) ) ;
#15787 = CARTESIAN_POINT ( 'NONE',  ( 61.65536943582333151, -1.983739999999999837, -11.98363747855214712 ) ) ;
#15786 = CARTESIAN_POINT ( 'NONE',  ( 3.777296294006362576, 11.64801722256006045, 2.252079683228215057 ) ) ;
#15788 = ORIENTED_EDGE ( 'NONE', *, *, #12609, .F. ) ;
#15789 = CARTESIAN_POINT ( 'NONE',  ( 1.952969610814715207, 8.739187247087119914, 8.731249999999999289 ) ) ;
#15790 = ORIENTED_EDGE ( 'NONE', *, *, #165, .F. ) ;
#15791 = CARTESIAN_POINT ( 'NONE',  ( 19.41351574269321389, 0.4248733107149043620, -14.98634048918820483 ) ) ;
#15792 = ADVANCED_FACE ( 'NONE', ( #9376 ), #10033, .T. ) ;
#15793 = EDGE_CURVE ( 'NONE', #14145, #12588, #8967, .T. ) ;
#15794 = CARTESIAN_POINT ( 'NONE',  ( 14.56131799329373600, -7.268434166347159220, -16.34826698112718901 ) ) ;
#15795 = VERTEX_POINT ( 'NONE', #16469 ) ;
#15796 = FACE_OUTER_BOUND ( 'NONE', #4309, .T. ) ;
#15797 = CIRCLE ( 'NONE', #7318, 1.984375000000000000 ) ;
#15798 = CARTESIAN_POINT ( 'NONE',  ( 22.04181838752732148, 16.26393749999999727, 0.06645525512612464325 ) ) ;
#15799 = CARTESIAN_POINT ( 'NONE',  ( 39.07078961959606289, -4.569743463999999200, -27.14892015257980162 ) ) ;
#15800 = ORIENTED_EDGE ( 'NONE', *, *, #1837, .F. ) ;
#15801 = DIRECTION ( 'NONE',  ( 0.000000000000000000, 1.000000000000000000, 0.000000000000000000 ) ) ;
#15802 = DIRECTION ( 'NONE',  ( 0.000000000000000000, 1.000000000000000000, 0.000000000000000000 ) ) ;
#15803 = LINE ( 'NONE', #5601, #19727 ) ;
#15805 = CARTESIAN_POINT ( 'NONE',  ( -47.86112874365709047, -10.87373999999999974, -23.29368419115692035 ) ) ;
#15804 = DIRECTION ( 'NONE',  ( 0.000000000000000000, 1.000000000000000000, 0.000000000000000000 ) ) ;
#15806 = ORIENTED_EDGE ( 'NONE', *, *, #8812, .F. ) ;
#15807 = ORIENTED_EDGE ( 'NONE', *, *, #13582, .T. ) ;
#15809 = CARTESIAN_POINT ( 'NONE',  ( -46.55773479047372376, -5.714999999999999858, -7.870535429687039120 ) ) ;
#15808 = CARTESIAN_POINT ( 'NONE',  ( 4.177528246928537747, 11.26628406262684301, 1.990635909573889473 ) ) ;
#15810 = ORIENTED_EDGE ( 'NONE', *, *, #10074, .T. ) ;
#15812 = CARTESIAN_POINT ( 'NONE',  ( 10.83746537706882229, -3.114666494210958980, -16.41844068122003009 ) ) ;
#15811 = CARTESIAN_POINT ( 'NONE',  ( 4.811567550396895321, 11.20075355227730185, 4.778909014656798071 ) ) ;
#15813 = ORIENTED_EDGE ( 'NONE', *, *, #13843, .F. ) ;
#15814 = AXIS2_PLACEMENT_3D ( 'NONE', #20395, #523, #5487 ) ;
#15815 = ORIENTED_EDGE ( 'NONE', *, *, #8029, .T. ) ;
#15816 = CARTESIAN_POINT ( 'NONE',  ( 1.300001150583172116, 13.18543556399213124, 7.424019162913821468 ) ) ;
#15817 = EDGE_CURVE ( 'NONE', #16263, #6310, #18120, .T. ) ;
#15818 = EDGE_LOOP ( 'NONE', ( #2194, #11111, #846, #7677 ) ) ;
#15819 = FACE_OUTER_BOUND ( 'NONE', #19757, .T. ) ;
#15820 = DIRECTION ( 'NONE',  ( 0.000000000000000000, 1.000000000000000000, 0.000000000000000000 ) ) ;
#15821 = DIRECTION ( 'NONE',  ( 0.000000000000000000, 0.000000000000000000, -1.000000000000000000 ) ) ;
#15822 = CARTESIAN_POINT ( 'NONE',  ( 29.64606458365116737, -7.547927499999999235, -15.53894806404596096 ) ) ;
#15823 = CARTESIAN_POINT ( 'NONE',  ( 3.602201510832755638, 16.49131183736701800, 9.203092360088074741 ) ) ;
#15824 = AXIS2_PLACEMENT_3D ( 'NONE', #1648, #3004, #15163 ) ;
#15825 = ORIENTED_EDGE ( 'NONE', *, *, #1487, .F. ) ;
#15826 = CARTESIAN_POINT ( 'NONE',  ( 5.691239657922468886, 14.17727879546418812, 7.604247685195596240 ) ) ;
#15827 = DIRECTION ( 'NONE',  ( -0.000000000000000000, -1.000000000000000000, 0.000000000000000000 ) ) ;
#15828 = CARTESIAN_POINT ( 'NONE',  ( 9.335363283976800375, 36.51313500000000545, -14.20581391854862474 ) ) ;
#15829 = DIRECTION ( 'NONE',  ( -0.9579671649362033747, 0.000000000000000000, 0.2868778675745011220 ) ) ;
#15830 = LINE ( 'NONE', #2655, #12687 ) ;
#15831 = ORIENTED_EDGE ( 'NONE', *, *, #4511, .T. ) ;
#15832 = ORIENTED_EDGE ( 'NONE', *, *, #6461, .T. ) ;
#15833 = CARTESIAN_POINT ( 'NONE',  ( 10.22892371477560403, 21.50410229886458424, 0.3058668854873597964 ) ) ;
#15834 = CARTESIAN_POINT ( 'NONE',  ( 29.01020070778135818, -14.84248999999999974, -13.85841188422236492 ) ) ;
#15835 = CARTESIAN_POINT ( 'NONE',  ( 11.63891272997743442, 10.83756077274092355, -0.7463790179119675905 ) ) ;
#15836 = ORIENTED_EDGE ( 'NONE', *, *, #20457, .T. ) ;
#15837 = ORIENTED_EDGE ( 'NONE', *, *, #9724, .T. ) ;
#15838 = DIRECTION ( 'NONE',  ( -0.2868778675745010664, 0.000000000000000000, -0.9579671649362032637 ) ) ;
#15839 = CARTESIAN_POINT ( 'NONE',  ( 7.255630842477019726, 16.46413444789888558, -2.887487180789374719 ) ) ;
#15840 = DIRECTION ( 'NONE',  ( 0.000000000000000000, 0.000000000000000000, 1.000000000000000000 ) ) ;
#15841 = DIRECTION ( 'NONE',  ( -0.2490110332224850509, 0.000000000000000000, 0.9685006480810792739 ) ) ;
#15842 = CARTESIAN_POINT ( 'NONE',  ( 5.601911010437768290, 14.57750533428744255, -1.041327773958115710 ) ) ;
#15843 = ADVANCED_FACE ( 'NONE', ( #5942 ), #1301, .F. ) ;
#15844 = VECTOR ( 'NONE', #8634, 1000.000000000000000 ) ;
#15845 = CARTESIAN_POINT ( 'NONE',  ( 1.868540122251793001, 20.38723677272791690, 4.979979739744280209 ) ) ;
#15846 = DIRECTION ( 'NONE',  ( 0.000000000000000000, 1.000000000000000000, 0.000000000000000000 ) ) ;
#15847 = CARTESIAN_POINT ( 'NONE',  ( 13.96517196999903376, 21.80725978669622123, 2.219877022834359170 ) ) ;
#15848 = CARTESIAN_POINT ( 'NONE',  ( 4.883189917998404184, 12.13604628887379100, 5.162602853463313046 ) ) ;
#15849 = CARTESIAN_POINT ( 'NONE',  ( 6.256221673970314257, 10.85576871210978211, 2.354533235149611770 ) ) ;
#15850 = CARTESIAN_POINT ( 'NONE',  ( 0.4262966382305843349, 20.71823079690684466, 6.782306411708023397 ) ) ;
#15851 = DIRECTION ( 'NONE',  ( 0.000000000000000000, 1.000000000000000000, 0.000000000000000000 ) ) ;
#15852 = CARTESIAN_POINT ( 'NONE',  ( 3.341519096695713564, 13.61484622919644139, 7.613859718236023255 ) ) ;
#15853 = DIRECTION ( 'NONE',  ( 0.7532174416907898573, 0.000000000000000000, 0.6577716059034334206 ) ) ;
#15854 = DIRECTION ( 'NONE',  ( 0.000000000000000000, -1.000000000000000000, 0.000000000000000000 ) ) ;
#15855 = CARTESIAN_POINT ( 'NONE',  ( 20.67432262747533045, -1.268898791072118559, -14.02093111710477658 ) ) ;
#15856 = CARTESIAN_POINT ( 'NONE',  ( 30.24348838687780727, -1.983739999999999837, -20.27293523655082552 ) ) ;
#15857 = CARTESIAN_POINT ( 'NONE',  ( 21.03437500000000071, 1.984375000000000000, 5.159374999999999822 ) ) ;
#15858 = CARTESIAN_POINT ( 'NONE',  ( 10.70904873084618281, 10.90722994128907253, 3.871866132961096163 ) ) ;
#15859 = VERTEX_POINT ( 'NONE', #21419 ) ;
#15860 = EDGE_CURVE ( 'NONE', #4521, #16037, #21092, .T. ) ;
#15861 = B_SPLINE_SURFACE_WITH_KNOTS ( 'NONE', 3, 3, ( 
 ( #12921, #19631, #20055, #13250, #1388, #16866, #6486, #20161, #8351, #3161, #11464, #21839, #51, #16769, #15122, #18412, #9893, #1711, #6912, #16971, #1821, #20375, #19959, #3062, #6693, #169, #8564, #13453, #8130, #9785, #21737, #1608, #5038, #4831, #18210, #3387, #15340, #13675, #16554, #14909, #6805, #11566, #8247, #5141, #18303, #13351, #21625, #1501, #16658, #15019, #6590, #4925, #11673, #15223, #10016, #3283, #11789, #18521, #13565, #10120, #8450, #20269, #11893, #18621, #3488, #10224, #20488 ),
 ( #17191, #2379, #12331, #2265, #17423, #17301, #5571, #14013, #7140, #2148, #502, #3600, #15674, #19057, #9106, #8892, #15887, #20605, #275, #3710, #13908, #8674, #5691, #18733, #7253, #1930, #17531, #712, #4040, #15556, #12225, #5240, #15781, #9005, #10786, #10452, #10342, #7462, #14233, #607, #20716, #7015, #17085, #12120, #15448, #19176, #3932, #7351, #10676, #20824, #5357, #5463, #14118, #12001, #13782, #18844, #2031, #8775, #18948, #387, #12452, #3821, #10555, #14335, #4671, #18160, #7574 ),
 ( #9633, #21051, #5903, #21455, #1446, #829, #4554, #16399, #12562, #11411, #3222, #3014, #12977, #8301, #4148, #8194, #19685, #10886, #11293, #18356, #16001, #9217, #16501, #1236, #18044, #14966, #19286, #21569, #2900, #9960, #6427, #18253, #11510, #9739, #13197, #8078, #7977, #1337, #14853, #17634, #19906, #4780, #16719, #3112, #1557, #14749, #6312, #13086, #19792, #2486, #21683, #9838, #16608, #6543, #11620, #20951, #20007, #13304, #4876, #5807, #3657, #12061, #10069, #10281, #6865, #224, #13624 ),
 ( #20323, #18788, #15402, #3543, #10402, #17147, #15289, #18471, #11846, #1987, #17031, #3439, #5193, #8728, #1877, #15504, #16818, #11946, #10173, #1763, #1658, #4981, #20427, #5097, #18900, #18673, #8625, #13399, #6964, #18574, #16916, #8397, #12176, #332, #3339, #6749, #7077, #13730, #13844, #15073, #11738, #20549, #5411, #3772, #5295, #10507, #17251, #2093, #21787, #6634, #115, #15171, #8509, #20109, #2, #13515, #20223, #2545, #17584, #17694, #3882, #5755, #3991, #17478, #10619, #20663, #14287 ),
 ( #5954, #11057, #21005, #10835, #17369, #5521, #15731, #19006, #885, #19234, #12610, #5852, #9278, #8952, #2323, #2436, #12718, #15614, #4317, #559, #21102, #659, #19443, #12510, #16053, #13964, #2213, #14179, #4096, #7303, #12282, #7626, #17812, #19121, #14067, #20774, #9056, #10938, #5636, #12396, #10735, #452, #20884, #8837, #9161, #15833, #7203, #7406, #14388, #15945, #773, #7525, #19335, #4202, #12842, #19765, #12953, #17912, #4755, #982, #2990, #14617, #21658, #9715, #21540, #14828, #14725 ),
 ( #16372, #13170, #13280, #11162, #6185, #19986, #11267, #18132, #11598, #11386, #6520, #14943, #19881, #7953, #6285, #9605, #1097, #6401, #4857, #8165, #2658, #9388, #2759, #16155, #13060, #7733, #14494, #4640, #21212, #6070, #19660, #21431, #16479, #9494, #19563, #1313, #4431, #16265, #7840, #21324, #11491, #4528, #18014, #18235, #2873, #1210, #8056, #3092, #9818, #16586, #1422, #1533, #5073, #199, #16894, #306, #5170, #8375, #20404, #11921, #8277, #3316, #5271, #20522, #18651, #15376, #11710 ),
 ( #13600, #3520, #8600, #15048, #10256, #11823, #16796, #10047, #10149, #6941, #7049, #4955, #21870, #13816, #18552, #17004, #5389, #1857, #18335, #8701, #15149, #3196, #1744, #15263, #16693, #8483, #6724, #13486, #18445, #15480, #12031, #6614, #1635, #13704, #18765, #3634, #9930, #21762, #10376, #17123, #13379, #90, #1963, #20088, #6841, #20202, #3416, #20301, #10481, #421, #8927, #18979, #7173, #5495, #532, #3853, #7281, #17223, #12257, #13938, #20635, #2065, #3748, #2185, #8806, #10591, #17337 ),
 ( #15704, #20749, #15582, #14042, #5606, #12366, #12153, #18877, #7129, #12219, #265, #11994, #5029, #21831, #16857, #20153, #2022, #20366, #13774, #15437, #3703, #10111, #18613, #18722, #13898, #16761, #5455, #1702, #378, #1812, #20597, #6901, #17183, #15113, #3379, #15333, #13665, #18512, #6686, #8765, #18938, #20261, #8443, #15214, #10216, #12110, #11780, #43, #5133, #1600, #158, #10008, #5231, #6796, #8342, #13445, #18835, #13556, #11885, #3479, #16963, #8556, #3592, #10333, #17077, #1920, #10444 ),
 ( #8665, #7007, #20477, #5347, #15547, #12443, #2258, #10667, #17521, #14329, #14430, #12320, #7344, #21147, #19171, #19277, #12773, #12554, #7670, #16097, #15773, #6000, #2369, #702, #2140, #9097, #14110, #599, #19047, #926, #12655, #14006, #17416, #7568, #10877, #21046, #3810, #15665, #19382, #5894, #10545, #15876, #821, #4137, #14222, #4250, #10986, #4034, #7247, #20815, #17742, #20940, #5681, #7449, #2590, #17627, #9325, #20708, #5799, #2480, #9208, #15991, #494, #17293, #10777, #8995, #8883 ) ),
 .UNSPECIFIED., .F., .F., .F.,
 ( 4, 1, 1, 1, 1, 1, 4 ),
 ( 4, 1, 1, 1, 1, 1, 1, 1, 1, 1, 1, 1, 1, 1, 1, 1, 1, 1, 1, 1, 1, 1, 1, 1, 1, 1, 1, 1, 1, 1, 1, 1, 1, 1, 1, 1, 1, 1, 1, 1, 1, 1, 1, 1, 1, 1, 1, 1, 1, 1, 1, 1, 1, 1, 1, 1, 1, 1, 1, 1, 1, 1, 1, 1, 4 ),
 ( 0.4887878733748999838, 0.5000000000000000000, 0.6250000000000000000, 0.7500000000000000000, 0.8750000000000000000, 1.000000000000000000, 1.011212126625000041 ),
 ( -0.02000000000000000042, -0.003749999999999999861, 0.01250000000000000069, 0.02875000000000000125, 0.04499999999999999833, 0.06124999999999999889, 0.07749999999999999944, 0.09375000000000000000, 0.1100000000000000006, 0.1262500000000000011, 0.1424999999999999878, 0.1587500000000000022, 0.1749999999999999889, 0.1912500000000000033, 0.2074999999999999900, 0.2237500000000000044, 0.2399999999999999911, 0.2562499999999999778, 0.2725000000000000200, 0.2887500000000000067, 0.3049999999999999933, 0.3212499999999999800, 0.3375000000000000222, 0.3537500000000000089, 0.3699999999999999956, 0.3862499999999999822, 0.4025000000000000244, 0.4187500000000000111, 0.4349999999999999978, 0.4512499999999999845, 0.4675000000000000266, 0.4837500000000000133, 0.5000000000000000000, 0.5162499999999999867, 0.5324999999999999734, 0.5487499999999999600, 0.5649999999999999467, 0.5812500000000000444, 0.5975000000000000311, 0.6137500000000000178, 0.6300000000000000044, 0.6462499999999999911, 0.6624999999999999778, 0.6787499999999999645, 0.6949999999999999512, 0.7112500000000000488, 0.7275000000000000355, 0.7437500000000000222, 0.7600000000000000089, 0.7762499999999999956, 0.7924999999999999822, 0.8087499999999999689, 0.8249999999999999556, 0.8412500000000000533, 0.8575000000000000400, 0.8737500000000000266, 0.8900000000000000133, 0.9062500000000000000, 0.9224999999999999867, 0.9387499999999999734, 0.9549999999999999600, 0.9712499999999999467, 0.9875000000000000444, 1.003749999999999920, 1.020000000000000018 ),
 .UNSPECIFIED. ) ;
#15862 = DIRECTION ( 'NONE',  ( 0.3542738219355867080, 0.000000000000000000, 0.9351417320872553729 ) ) ;
#15863 = CARTESIAN_POINT ( 'NONE',  ( 11.43322488496470157, 12.38805227212553106, -1.775723318043512799 ) ) ;
#15864 = CARTESIAN_POINT ( 'NONE',  ( 5.364804770603153194, 14.99291397360876132, -1.985349221369826500 ) ) ;
#15865 = PLANE ( 'NONE',  #21850 ) ;
#15866 = CARTESIAN_POINT ( 'NONE',  ( 3.267967622520437931, 13.61749910441900191, 7.632369304580858937 ) ) ;
#15867 =( GEOMETRIC_REPRESENTATION_CONTEXT ( 3 ) GLOBAL_UNCERTAINTY_ASSIGNED_CONTEXT ( ( #5460 ) ) GLOBAL_UNIT_ASSIGNED_CONTEXT ( ( #19516, #12906, #4267 ) ) REPRESENTATION_CONTEXT ( 'NONE', 'WORKASPACE' ) );
#15868 = ORIENTED_EDGE ( 'NONE', *, *, #15972, .F. ) ;
#15869 = FACE_OUTER_BOUND ( 'NONE', #16289, .T. ) ;
#15870 = EDGE_CURVE ( 'NONE', #19449, #10001, #12708, .T. ) ;
#15871 = ADVANCED_FACE ( 'NONE', ( #14376 ), #4626, .F. ) ;
#15872 = DIRECTION ( 'NONE',  ( 0.000000000000000000, 1.000000000000000000, 0.000000000000000000 ) ) ;
#15873 = ORIENTED_EDGE ( 'NONE', *, *, #11200, .F. ) ;
#15874 = CARTESIAN_POINT ( 'NONE',  ( 9.425691308541154001, 13.73439867555944716, -2.265729419357018326 ) ) ;
#15875 = CARTESIAN_POINT ( 'NONE',  ( 4.909756017696536468, 18.80479460024974614, 7.293209006630767099 ) ) ;
#15876 = CARTESIAN_POINT ( 'NONE',  ( 9.290483991089809379, 15.41846441754162456, -2.879978118279780563 ) ) ;
#15877 = CARTESIAN_POINT ( 'NONE',  ( 46.03750000000000142, 1.984375000000000000, -10.31874999999999964 ) ) ;
#15878 = CARTESIAN_POINT ( 'NONE',  ( 2.761194845577150669, 20.74767509450332170, 6.499773152090608797 ) ) ;
#15879 = LINE ( 'NONE', #3926, #14246 ) ;
#15880 = DIRECTION ( 'NONE',  ( -0.3542738219355896501, 0.000000000000000000, -0.9351417320872542627 ) ) ;
#15881 = VECTOR ( 'NONE', #21791, 1000.000000000000114 ) ;
#15882 = CARTESIAN_POINT ( 'NONE',  ( 12.69615196668531709, -0.5037659573396899848, -16.49031973222839298 ) ) ;
#15883 = UNCERTAINTY_MEASURE_WITH_UNIT (LENGTH_MEASURE( 1.000000000000000082E-05 ), #17409, 'distance_accuracy_value', 'NONE');
#15884 = CARTESIAN_POINT ( 'NONE',  ( 54.11611804786240043, 32.54502000000000095, -30.58983753981140197 ) ) ;
#15885 = ORIENTED_EDGE ( 'NONE', *, *, #16755, .T. ) ;
#15886 = CARTESIAN_POINT ( 'NONE',  ( 11.18338078536718427, 16.32796899754609043, 6.823261089681437852 ) ) ;
#15887 = CARTESIAN_POINT ( 'NONE',  ( 9.538671442711894599, 14.64581734927065249, 7.844515866693947181 ) ) ;
#15888 = ADVANCED_FACE ( 'NONE', ( #14483 ), #16253, .F. ) ;
#15889 = CARTESIAN_POINT ( 'NONE',  ( 39.26944594349237150, -5.166360000000000063, -4.208320303602718582 ) ) ;
#15890 = ORIENTED_EDGE ( 'NONE', *, *, #20190, .F. ) ;
#15891 = CARTESIAN_POINT ( 'NONE',  ( 10.41107459178117978, 11.41251432934954302, 2.646321841035150335 ) ) ;
#15892 = AXIS2_PLACEMENT_3D ( 'NONE', #17780, #7492, #954 ) ;
#15893 = PLANE ( 'NONE',  #10620 ) ;
#15894 = CARTESIAN_POINT ( 'NONE',  ( 0.5564837971381878523, 19.70421451463541018, 7.041132247275984746 ) ) ;
#15896 = PLANE ( 'NONE',  #13830 ) ;
#15895 = CARTESIAN_POINT ( 'NONE',  ( 1.456693750638721641, 13.27625335140768215, 0.8154936714224948480 ) ) ;
#15897 = EDGE_LOOP ( 'NONE', ( #4184, #15937 ) ) ;
#15898 = CARTESIAN_POINT ( 'NONE',  ( 7.532599918355038504, 15.95844914551919302, 8.384485894956869245 ) ) ;
#15899 = DIRECTION ( 'NONE',  ( -0.1831666983862943188, 0.000000000000000000, 0.9830818687180962190 ) ) ;
#15900 = DIRECTION ( 'NONE',  ( -0.8943161143440100380, 0.000000000000000000, -0.4474356798743612806 ) ) ;
#15901 = VECTOR ( 'NONE', #937, 1000.000000000000000 ) ;
#15902 = ORIENTED_EDGE ( 'NONE', *, *, #16161, .T. ) ;
#15903 = EDGE_CURVE ( 'NONE', #12014, #2636, #13581, .T. ) ;
#15904 = CARTESIAN_POINT ( 'NONE',  ( 2.063750000000000195, 30.16440499999999858, 8.335010000000000474 ) ) ;
#15905 = CARTESIAN_POINT ( 'NONE',  ( 11.65751173500739846, -3.109302012046705421, -17.03197226462303249 ) ) ;
#15906 = VERTEX_POINT ( 'NONE', #6059 ) ;
#15907 = DIRECTION ( 'NONE',  ( 1.000000000000000000, 0.000000000000000000, 0.000000000000000000 ) ) ;
#15908 = EDGE_CURVE ( 'NONE', #19333, #1356, #7942, .T. ) ;
#15909 = ADVANCED_BREP_SHAPE_REPRESENTATION ( '', ( #6575, #2234 ), #15867 ) ;
#15910 = DIRECTION ( 'NONE',  ( -0.2490110332224850231, 0.000000000000000000, 0.9685006480810791629 ) ) ;
#15911 = CARTESIAN_POINT ( 'NONE',  ( 1.854799496439154316, 19.43893749999999798, 3.211081754263136911 ) ) ;
#15912 = VERTEX_POINT ( 'NONE', #21313 ) ;
#15913 = AXIS2_PLACEMENT_3D ( 'NONE', #1844, #8585, #15359 ) ;
#15914 = CARTESIAN_POINT ( 'NONE',  ( 29.15193331460030279, -6.752907499999998286, -13.61707959051006966 ) ) ;
#15915 = ADVANCED_FACE ( 'NONE', ( #6174 ), #1199, .T. ) ;
#15917 = FACE_OUTER_BOUND ( 'NONE', #15478, .T. ) ;
#15916 = CARTESIAN_POINT ( 'NONE',  ( -21.45091887247874851, -8.248365470396340271, -9.992285829511605044 ) ) ;
#15918 = ORIENTED_EDGE ( 'NONE', *, *, #15776, .T. ) ;
#15919 = EDGE_CURVE ( 'NONE', #16810, #14694, #9017, .T. ) ;
#15920 = ORIENTED_EDGE ( 'NONE', *, *, #15367, .F. ) ;
#15921 = ADVANCED_FACE ( 'NONE', ( #14453 ), #946, .F. ) ;
#15923 = CARTESIAN_POINT ( 'NONE',  ( 13.28822531734660828, -3.968114999999999615, -15.23578611614444078 ) ) ;
#15922 = CARTESIAN_POINT ( 'NONE',  ( 5.595233681759747668, 13.84461567157916662, 8.302901642620097888 ) ) ;
#15924 = VERTEX_POINT ( 'NONE', #19400 ) ;
#15925 = CARTESIAN_POINT ( 'NONE',  ( 5.363079780418651410, 12.55216059408865092, 7.235226968914967749 ) ) ;
#15926 = ORIENTED_EDGE ( 'NONE', *, *, #20509, .T. ) ;
#15927 = CIRCLE ( 'NONE', #2484, 25.00312500000000426 ) ;
#15928 = ORIENTED_EDGE ( 'NONE', *, *, #1905, .T. ) ;
#15929 = ORIENTED_EDGE ( 'NONE', *, *, #7059, .F. ) ;
#15930 = AXIS2_PLACEMENT_3D ( 'NONE', #20793, #9186, #8859 ) ;
#15931 = AXIS2_PLACEMENT_3D ( 'NONE', #14906, #21622, #18098 ) ;
#15932 = FACE_OUTER_BOUND ( 'NONE', #7564, .T. ) ;
#15933 = LINE ( 'NONE', #7292, #12150 ) ;
#15934 = DIRECTION ( 'NONE',  ( 0.000000000000000000, 0.000000000000000000, 1.000000000000000000 ) ) ;
#15935 = CARTESIAN_POINT ( 'NONE',  ( 2.461191507070185303, 20.72975021207655288, 6.582046662092221112 ) ) ;
#15936 = CARTESIAN_POINT ( 'NONE',  ( 20.09790673380831905, -2.779220565229514772, -15.34579478154137711 ) ) ;
#15937 = ORIENTED_EDGE ( 'NONE', *, *, #14628, .T. ) ;
#15938 = CARTESIAN_POINT ( 'NONE',  ( 1.904212788493860220, 17.24875406955469259, 9.107061817004916904 ) ) ;
#15939 = CARTESIAN_POINT ( 'NONE',  ( 10.86025044861609601, -4.788864733524861528, -16.24762125301678850 ) ) ;
#15940 = CARTESIAN_POINT ( 'NONE',  ( -20.63749999999999929, 16.27314499999999953, 8.731249999999999289 ) ) ;
#15941 = CARTESIAN_POINT ( 'NONE',  ( -3.037751992662818257, 3.961447500000001565, -30.02724401157551526 ) ) ;
#15942 = VERTEX_POINT ( 'NONE', #5915 ) ;
#15943 = EDGE_CURVE ( 'NONE', #8700, #6063, #14350, .T. ) ;
#15944 = VERTEX_POINT ( 'NONE', #17769 ) ;
#15945 = CARTESIAN_POINT ( 'NONE',  ( 12.57069057875543550, 18.63767531088674190, 6.547553293110945027 ) ) ;
#15947 = FACE_OUTER_BOUND ( 'NONE', #5192, .T. ) ;
#15946 = FACE_OUTER_BOUND ( 'NONE', #2941, .T. ) ;
#15948 = CARTESIAN_POINT ( 'NONE',  ( 13.38722737856375744, 14.77849355198858206, 6.969650373707040991 ) ) ;
#15949 = ORIENTED_EDGE ( 'NONE', *, *, #20068, .T. ) ;
#15950 = VERTEX_POINT ( 'NONE', #7589 ) ;
#15951 = DIRECTION ( 'NONE',  ( -0.2490110332224850509, 0.000000000000000000, 0.9685006480810792739 ) ) ;
#15952 = CARTESIAN_POINT ( 'NONE',  ( 7.281201052484665759, 13.72469829375204675, -2.239932892534894471 ) ) ;
#15953 = CARTESIAN_POINT ( 'NONE',  ( 7.318285782056717537, 16.58796963715414208, 7.711759744564571584 ) ) ;
#15954 = DIRECTION ( 'NONE',  ( 0.000000000000000000, -1.000000000000000000, -0.000000000000000000 ) ) ;
#15955 = CARTESIAN_POINT ( 'NONE',  ( 9.153486460148078763, 17.16681038731015008, 7.158488902892022665 ) ) ;
#15956 = CARTESIAN_POINT ( 'NONE',  ( 7.289870466149695361, 14.17692335100063161, 7.110251240425253805 ) ) ;
#15957 = AXIS2_PLACEMENT_3D ( 'NONE', #13656, #6574, #6787 ) ;
#15958 = CIRCLE ( 'NONE', #13474, 2.381250000000001421 ) ;
#15959 = AXIS2_PLACEMENT_3D ( 'NONE', #8108, #9665, #3045 ) ;
#15960 = CARTESIAN_POINT ( 'NONE',  ( 38.99880687437181592, 40.07783883761410237, -3.901390339950522090 ) ) ;
#15961 = CARTESIAN_POINT ( 'NONE',  ( 7.199513328304186999, 11.36662928180900245, 4.932186602622403271 ) ) ;
#15962 = CARTESIAN_POINT ( 'NONE',  ( 5.134883484631279416, 19.21498006567040306, 8.078918003304201179 ) ) ;
#15963 = CARTESIAN_POINT ( 'NONE',  ( 1.548165812409910025, 17.46078721926186361, 9.485929473351337293 ) ) ;
#15964 = PLANE ( 'NONE',  #15302 ) ;
#15965 = CARTESIAN_POINT ( 'NONE',  ( 1.883633422024908022, 16.41907190720915466, -0.01618598629114483337 ) ) ;
#15966 = CARTESIAN_POINT ( 'NONE',  ( 12.38912331111999343, -14.84248999999999974, 5.137219823516766759 ) ) ;
#15967 = LINE ( 'NONE', #19258, #19474 ) ;
#15968 = CARTESIAN_POINT ( 'NONE',  ( 20.88674645337222202, -2.120330402937725012, -13.93411895024804359 ) ) ;
#15969 = VECTOR ( 'NONE', #14055, 1000.000000000000000 ) ;
#15970 = VERTEX_POINT ( 'NONE', #2614 ) ;
#15971 = DIRECTION ( 'NONE',  ( 0.000000000000000000, 1.000000000000000000, 0.000000000000000000 ) ) ;
#15972 = EDGE_CURVE ( 'NONE', #20891, #11142, #14026, .T. ) ;
#15973 = VECTOR ( 'NONE', #16497, 1000.000000000000227 ) ;
#15974 = CIRCLE ( 'NONE', #18064, 1.587499999999999911 ) ;
#15975 = CARTESIAN_POINT ( 'NONE',  ( 11.42442798422983685, 14.30946655864417671, 7.226238609427539039 ) ) ;
#15976 = ORIENTED_EDGE ( 'NONE', *, *, #2696, .T. ) ;
#15977 = CYLINDRICAL_SURFACE ( 'NONE', #754, 0.7950199999999998379 ) ;
#15978 = VECTOR ( 'NONE', #7834, 1000.000000000000114 ) ;
#15979 = CARTESIAN_POINT ( 'NONE',  ( 11.49429421792066996, 18.69515674907532699, -3.066687557635257910 ) ) ;
#15980 = CARTESIAN_POINT ( 'NONE',  ( 5.377061541145786272, 14.53036832121391164, -1.845926119401802623 ) ) ;
#15981 = CARTESIAN_POINT ( 'NONE',  ( 30.24348838687780727, 0.000000000000000000, -20.27293523655082552 ) ) ;
#15982 = CARTESIAN_POINT ( 'NONE',  ( 1.878793507312973787, 13.53433865536812064, 1.020842242705974678 ) ) ;
#15983 = VERTEX_POINT ( 'NONE', #7692 ) ;
#15984 = SURFACE_SIDE_STYLE ('',( #12435 ) ) ;
#15985 = FACE_OUTER_BOUND ( 'NONE', #19687, .T. ) ;
#15986 = CIRCLE ( 'NONE', #1483, 0.7950200000000003930 ) ;
#15987 = AXIS2_PLACEMENT_3D ( 'NONE', #9812, #18231, #16259 ) ;
#15988 = VECTOR ( 'NONE', #20752, 1000.000000000000114 ) ;
#15989 = VERTEX_POINT ( 'NONE', #20837 ) ;
#15990 = CARTESIAN_POINT ( 'NONE',  ( 7.540178019304795143, 16.36402550683704860, -2.249428100403033870 ) ) ;
#15991 = CARTESIAN_POINT ( 'NONE',  ( 11.75259991899696033, 19.71652463870320204, -2.548980710552388285 ) ) ;
#15992 = LINE ( 'NONE', #5895, #7852 ) ;
#15993 = CIRCLE ( 'NONE', #18776, 11.02160133116777985 ) ;
#15994 = MECHANICAL_DESIGN_GEOMETRIC_PRESENTATION_REPRESENTATION (  '', ( #1491 ), #8887 ) ;
#15995 = CARTESIAN_POINT ( 'NONE',  ( 53.14266576735298031, -7.546379553159687781, -16.66242751532464084 ) ) ;
#15996 = CARTESIAN_POINT ( 'NONE',  ( 5.276755280550131211, 18.51750724673628667, 8.329952144543302239 ) ) ;
#15997 = CARTESIAN_POINT ( 'NONE',  ( 55.33978576324753362, -1.983739999999999837, -23.05096232720518756 ) ) ;
#15998 = EDGE_CURVE ( 'NONE', #9031, #7389, #852, .T. ) ;
#15999 = EDGE_LOOP ( 'NONE', ( #15292, #17633, #14466, #5604 ) ) ;
#16000 = ADVANCED_FACE ( 'NONE', ( #12236 ), #18961, .F. ) ;
#16001 = CARTESIAN_POINT ( 'NONE',  ( 8.070802031145120736, 10.68384337266676276, 1.758507783024191973 ) ) ;
#16002 = CARTESIAN_POINT ( 'NONE',  ( 55.52866846859686234, 36.51313500000000545, -11.12083858657437752 ) ) ;
#16003 = CIRCLE ( 'NONE', #20205, 1.190625000000000488 ) ;
#16004 = ORIENTED_EDGE ( 'NONE', *, *, #7432, .T. ) ;
#16005 = CARTESIAN_POINT ( 'NONE',  ( 10.25666463770645365, 11.36678447621568289, 1.976058869409572205 ) ) ;
#16006 = CARTESIAN_POINT ( 'NONE',  ( 1.345153252091858542, 17.14040452170628370, 8.773309266493196645 ) ) ;
#16008 = CYLINDRICAL_SURFACE ( 'NONE', #5993, 0.7950199999999993938 ) ;
#16007 = CARTESIAN_POINT ( 'NONE',  ( 2.873840625336028243, 18.12196835462199829, 8.704036440046063916 ) ) ;
#16009 = VERTEX_POINT ( 'NONE', #3834 ) ;
#16010 = DIRECTION ( 'NONE',  ( 0.9784543669157944601, -0.000000000000000000, 0.2064631973582987945 ) ) ;
#16011 = CIRCLE ( 'NONE', #76, 4.365625000000000533 ) ;
#16012 = LINE ( 'NONE', #840, #8064 ) ;
#16013 = ORIENTED_EDGE ( 'NONE', *, *, #16838, .F. ) ;
#16014 = AXIS2_PLACEMENT_3D ( 'NONE', #15775, #7345, #19049 ) ;
#16015 = DIRECTION ( 'NONE',  ( -0.2490110332224850509, 0.000000000000000000, 0.9685006480810792739 ) ) ;
#16016 = CARTESIAN_POINT ( 'NONE',  ( 16.94878383384984488, 1.210823707880592348, -15.13240640632768041 ) ) ;
#16017 = ORIENTED_EDGE ( 'NONE', *, *, #9973, .F. ) ;
#16018 = CARTESIAN_POINT ( 'NONE',  ( 32.18388890846549799, -4.569743463999999200, 1.507793899792891468 ) ) ;
#16019 = ADVANCED_FACE ( 'NONE', ( #10569 ), #15686, .F. ) ;
#16020 = CIRCLE ( 'NONE', #4005, 20.83593750000000000 ) ;
#16021 = DIRECTION ( 'NONE',  ( 0.000000000000000000, 1.000000000000000000, 0.000000000000000000 ) ) ;
#16022 = DIRECTION ( 'NONE',  ( 0.000000000000000000, 0.000000000000000000, -1.000000000000000000 ) ) ;
#16023 = EDGE_CURVE ( 'NONE', #171, #7176, #5586, .T. ) ;
#16024 = VECTOR ( 'NONE', #16310, 1000.000000000000000 ) ;
#16025 = ORIENTED_EDGE ( 'NONE', *, *, #19165, .T. ) ;
#16026 = EDGE_CURVE ( 'NONE', #10001, #16893, #19070, .T. ) ;
#16027 = DIRECTION ( 'NONE',  ( -0.000000000000000000, -1.000000000000000000, 0.000000000000000000 ) ) ;
#16028 = EDGE_CURVE ( 'NONE', #11912, #736, #4513, .T. ) ;
#16029 = ORIENTED_EDGE ( 'NONE', *, *, #12764, .F. ) ;
#16031 = CYLINDRICAL_SURFACE ( 'NONE', #2864, 0.7950200000000003930 ) ;
#16030 = CARTESIAN_POINT ( 'NONE',  ( 7.541081845515885007, 16.64385683817606321, 8.488075708221099802 ) ) ;
#16032 = VERTEX_POINT ( 'NONE', #14684 ) ;
#16033 = CARTESIAN_POINT ( 'NONE',  ( 3.585433298076192710, 13.67760018920084164, -0.7025886874450966157 ) ) ;
#16034 = VERTEX_POINT ( 'NONE', #2945 ) ;
#16035 = VERTEX_POINT ( 'NONE', #6473 ) ;
#16036 = AXIS2_PLACEMENT_3D ( 'NONE', #17158, #5423, #9178 ) ;
#16037 = VERTEX_POINT ( 'NONE', #11553 ) ;
#16038 = CARTESIAN_POINT ( 'NONE',  ( 2.957488341128261311, 12.27600719534943607, 5.634643733745038574 ) ) ;
#16039 = EDGE_CURVE ( 'NONE', #17975, #21188, #16641, .T. ) ;
#16040 = EDGE_CURVE ( 'NONE', #2429, #6204, #7797, .T. ) ;
#16041 = DIRECTION ( 'NONE',  ( 0.000000000000000000, 1.000000000000000000, 0.000000000000000000 ) ) ;
#16042 = AXIS2_PLACEMENT_3D ( 'NONE', #18461, #14956, #6532 ) ;
#16043 = CARTESIAN_POINT ( 'NONE',  ( 39.90351579496220324, 38.56174168182639761, -3.031484349533014377 ) ) ;
#16044 = CARTESIAN_POINT ( 'NONE',  ( -13.87568970999206108, -1.983739999999999393, -9.457638332870221376 ) ) ;
#16045 = CARTESIAN_POINT ( 'NONE',  ( 2.892783912874654639, 11.35831051514739976, 5.278155357869695585 ) ) ;
#16046 = ORIENTED_EDGE ( 'NONE', *, *, #19326, .F. ) ;
#16047 = CARTESIAN_POINT ( 'NONE',  ( 7.614317487531611306, 16.59395432398027381, 7.713385099270380074 ) ) ;
#16048 = CARTESIAN_POINT ( 'NONE',  ( 8.781357490942916399, 39.28205249999999893, -18.85455479843708559 ) ) ;
#16049 = DIRECTION ( 'NONE',  ( 0.000000000000000000, 0.000000000000000000, -1.000000000000000000 ) ) ;
#16050 = CARTESIAN_POINT ( 'NONE',  ( 71.04062499999999147, 32.54502000000000095, -10.31874999999999964 ) ) ;
#16051 = EDGE_LOOP ( 'NONE', ( #13015, #19878, #7731, #12108 ) ) ;
#16052 = EDGE_LOOP ( 'NONE', ( #7411, #6040 ) ) ;
#16053 = CARTESIAN_POINT ( 'NONE',  ( 6.911024701182626018, 16.37218494104095967, -2.488299197932800855 ) ) ;
#16055 = LINE ( 'NONE', #21214, #9233 ) ;
#16054 = FACE_OUTER_BOUND ( 'NONE', #11250, .T. ) ;
#16056 = VECTOR ( 'NONE', #14784, 1000.000000000000114 ) ;
#16057 = CARTESIAN_POINT ( 'NONE',  ( 12.30817927592476835, 10.43710490882117981, 2.034649068642048864 ) ) ;
#16058 = ORIENTED_EDGE ( 'NONE', *, *, #11354, .F. ) ;
#16059 = EDGE_LOOP ( 'NONE', ( #17074, #1912, #814, #5225 ) ) ;
#16060 = LINE ( 'NONE', #7740, #6029 ) ;
#16061 = CARTESIAN_POINT ( 'NONE',  ( 7.885219324757854586, 20.04620933819776241, -1.563507728803273045 ) ) ;
#16062 = DIRECTION ( 'NONE',  ( -0.7421532822901579785, 0.000000000000000000, 0.6702301885068628895 ) ) ;
#16063 = DIRECTION ( 'NONE',  ( 0.000000000000000000, 1.000000000000000000, 0.000000000000000000 ) ) ;
#16064 = CARTESIAN_POINT ( 'NONE',  ( 7.753549000504421862, 20.82617040976970202, 3.772397917800740075 ) ) ;
#16065 = AXIS2_PLACEMENT_3D ( 'NONE', #8152, #5353, #21646 ) ;
#16066 = CARTESIAN_POINT ( 'NONE',  ( 2.082326296619658734, 20.28604016155938794, 5.534141863331107025 ) ) ;
#16067 = LINE ( 'NONE', #996, #12491 ) ;
#16068 = EDGE_CURVE ( 'NONE', #6310, #7268, #14568, .T. ) ;
#16069 = EDGE_CURVE ( 'NONE', #15912, #304, #6244, .T. ) ;
#16070 = CARTESIAN_POINT ( 'NONE',  ( 9.316887094131077518, 18.56746232396120533, 7.628866700226834219 ) ) ;
#16071 = AXIS2_PLACEMENT_3D ( 'NONE', #13410, #15081, #13312 ) ;
#16072 = DIRECTION ( 'NONE',  ( -0.2490110332224846346, 0.000000000000000000, 0.9685006480810792739 ) ) ;
#16073 = DIRECTION ( 'NONE',  ( 0.3542738219355867080, 0.000000000000000000, 0.9351417320872553729 ) ) ;
#16074 = CARTESIAN_POINT ( 'NONE',  ( 1.125632047368157584, 11.63764180229748213, 6.559284911491262804 ) ) ;
#16075 = CARTESIAN_POINT ( 'NONE',  ( 0.6387658443185789681, 11.44537632918167169, 4.316053075454154175 ) ) ;
#16076 = DIRECTION ( 'NONE',  ( 0.000000000000000000, 1.000000000000000000, 0.000000000000000000 ) ) ;
#16077 = CARTESIAN_POINT ( 'NONE',  ( 4.942683224323132229, 18.75934072859504198, 7.437106419775259880 ) ) ;
#16078 = CARTESIAN_POINT ( 'NONE',  ( 1.403477590199228464, 23.42690089012609178, 10.67779458928513314 ) ) ;
#16079 = CARTESIAN_POINT ( 'NONE',  ( 44.28293121686854761, -3.968114999999999615, -31.08068102505560759 ) ) ;
#16080 = AXIS2_PLACEMENT_3D ( 'NONE', #1436, #21443, #16280 ) ;
#16081 = ORIENTED_EDGE ( 'NONE', *, *, #20425, .T. ) ;
#16082 = DIRECTION ( 'NONE',  ( -0.8583349619704310207, 0.000000000000000000, 0.5130897514657826175 ) ) ;
#16083 = CARTESIAN_POINT ( 'NONE',  ( 11.39144718466197226, 13.80490758105914750, 7.009419656893866701 ) ) ;
#16084 = ORIENTED_EDGE ( 'NONE', *, *, #21754, .F. ) ;
#16085 = CARTESIAN_POINT ( 'NONE',  ( 29.36900889036359885, 1.958445551117574901, 10.71563714734171846 ) ) ;
#16086 = CARTESIAN_POINT ( 'NONE',  ( 5.424505126996017168, 13.78855881373742776, -1.522162338289739125 ) ) ;
#16087 = CARTESIAN_POINT ( 'NONE',  ( -23.81250000000000000, 16.27314499999999953, 8.731249999999999289 ) ) ;
#16088 = EDGE_LOOP ( 'NONE', ( #16759, #13254, #21606, #19546, #9896, #6913, #326 ) ) ;
#16089 = LINE ( 'NONE', #5888, #4985 ) ;
#16090 = DIRECTION ( 'NONE',  ( 0.000000000000000000, 1.000000000000000000, 0.000000000000000000 ) ) ;
#16091 = CIRCLE ( 'NONE', #2303, 0.5079999999999984528 ) ;
#16092 = EDGE_CURVE ( 'NONE', #8109, #16499, #16427, .T. ) ;
#16093 = CARTESIAN_POINT ( 'NONE',  ( 11.37333528896229851, 0.1854951822871341027, -16.98463289171863977 ) ) ;
#16094 = ORIENTED_EDGE ( 'NONE', *, *, #2193, .F. ) ;
#16095 = CARTESIAN_POINT ( 'NONE',  ( 8.491692939339465340, 11.40205806595764138, 1.750967937658206797 ) ) ;
#16096 = CARTESIAN_POINT ( 'NONE',  ( 5.299847422448394241, 16.73342696359956605, 8.025596137169321409 ) ) ;
#16097 = CARTESIAN_POINT ( 'NONE',  ( 8.610284304070962236, 11.53658052784436094, 3.528423034965584293 ) ) ;
#16098 = DIRECTION ( 'NONE',  ( -0.8609107660235850723, 0.000000000000000000, 0.5087559856598092844 ) ) ;
#16099 = DIRECTION ( 'NONE',  ( 0.000000000000000000, -1.000000000000000000, -0.000000000000000000 ) ) ;
#16100 = DIRECTION ( 'NONE',  ( -0.000000000000000000, -1.000000000000000000, 0.000000000000000000 ) ) ;
#16101 = CARTESIAN_POINT ( 'NONE',  ( 4.649021650351502721, 20.44826945341173641, 6.786196569202606277 ) ) ;
#16102 = CARTESIAN_POINT ( 'NONE',  ( 0.7843704457339527591, 25.39269750000000059, -23.55949434567611078 ) ) ;
#16103 = EDGE_LOOP ( 'NONE', ( #16390, #251, #14441, #10472 ) ) ;
#16104 = DIRECTION ( 'NONE',  ( -0.9129422336036127072, 0.000000000000000000, 0.4080888115384278536 ) ) ;
#16105 = EDGE_LOOP ( 'NONE', ( #18233, #2841, #309, #19949 ) ) ;
#16106 = CARTESIAN_POINT ( 'NONE',  ( 11.25455419701103921, 21.25597139212561260, 1.837441195538858763 ) ) ;
#16107 = DIRECTION ( 'NONE',  ( 0.000000000000000000, 1.000000000000000000, 0.000000000000000000 ) ) ;
#16108 = CARTESIAN_POINT ( 'NONE',  ( 0.3634868636840050682, 19.95706598340423099, 6.556391343133318728 ) ) ;
#16109 = CARTESIAN_POINT ( 'NONE',  ( 19.51141091471011180, 29.75832250000000201, -1.622220754415315547 ) ) ;
#16110 = ORIENTED_EDGE ( 'NONE', *, *, #10973, .T. ) ;
#16111 = DIRECTION ( 'NONE',  ( 0.9959941601142464629, 0.000000000000000000, 0.08941830359784717908 ) ) ;
#16112 = CARTESIAN_POINT ( 'NONE',  ( 30.78626241496060700, 23.40768749999999798, -2.552201779827368622 ) ) ;
#16113 = VERTEX_POINT ( 'NONE', #9876 ) ;
#16114 = CARTESIAN_POINT ( 'NONE',  ( 19.67909734877197891, 0.1298811790940870847, -14.89708569419555317 ) ) ;
#16115 = CARTESIAN_POINT ( 'NONE',  ( 0.4550004815227328137, 18.61582597019792118, 1.433257286243621920 ) ) ;
#16116 = EDGE_CURVE ( 'NONE', #4266, #20489, #4713, .T. ) ;
#16117 = CARTESIAN_POINT ( 'NONE',  ( 12.56520165224167584, -6.111738713647066668, -15.71496090202399110 ) ) ;
#16118 = VERTEX_POINT ( 'NONE', #1165 ) ;
#16119 = DIRECTION ( 'NONE',  ( 0.000000000000000000, -1.000000000000000000, -0.000000000000000000 ) ) ;
#16120 = CARTESIAN_POINT ( 'NONE',  ( 1.944368897882448266, 16.62334027767684930, 0.06855819222581667483 ) ) ;
#16121 = APPLICATION_CONTEXT ( 'automotive_design' ) ;
#16122 = CARTESIAN_POINT ( 'NONE',  ( -15.27935546639805331, 36.51313500000000545, -26.04713531390440906 ) ) ;
#16123 = ORIENTED_EDGE ( 'NONE', *, *, #8150, .F. ) ;
#16124 = DIRECTION ( 'NONE',  ( -0.9579671649362032637, 0.000000000000000000, 0.2868778675745010664 ) ) ;
#16126 = CARTESIAN_POINT ( 'NONE',  ( 29.64606458365116737, 36.49567249999999774, -15.53894806404596096 ) ) ;
#16125 = LINE ( 'NONE', #11025, #17623 ) ;
#16127 = ORIENTED_EDGE ( 'NONE', *, *, #11149, .T. ) ;
#16128 = VERTEX_POINT ( 'NONE', #12911 ) ;
#16129 = CARTESIAN_POINT ( 'NONE',  ( -15.39353573898878658, 37.13217763270220217, -10.30107656633069979 ) ) ;
#16131 = CARTESIAN_POINT ( 'NONE',  ( 44.27024749654656688, 38.88803500000000213, -8.722764363618033201 ) ) ;
#16130 = CARTESIAN_POINT ( 'NONE',  ( 0.8544710534764644594, 20.20188058797412012, 7.859027440807365927 ) ) ;
#16132 = ORIENTED_EDGE ( 'NONE', *, *, #21255, .F. ) ;
#16133 = CARTESIAN_POINT ( 'NONE',  ( 3.707196599236265211, 17.88651271022806100, -1.213880038145912721 ) ) ;
#16134 = ADVANCED_FACE ( 'NONE', ( #6024 ), #19946, .F. ) ;
#16135 = ORIENTED_EDGE ( 'NONE', *, *, #5765, .T. ) ;
#16136 = ORIENTED_EDGE ( 'NONE', *, *, #19951, .T. ) ;
#16137 = CARTESIAN_POINT ( 'NONE',  ( 0.9999235395336120158, 12.37449380620932260, 5.956091945474599747 ) ) ;
#16138 = EDGE_CURVE ( 'NONE', #3406, #4408, #11452, .T. ) ;
#16139 = ORIENTED_EDGE ( 'NONE', *, *, #5898, .F. ) ;
#16140 = EDGE_CURVE ( 'NONE', #10152, #18076, #8660, .T. ) ;
#16141 = EDGE_CURVE ( 'NONE', #14694, #5229, #5808, .T. ) ;
#16142 = CYLINDRICAL_SURFACE ( 'NONE', #14927, 1.191259999999999319 ) ;
#16143 = DIRECTION ( 'NONE',  ( -0.7421532822901579785, 0.000000000000000000, 0.6702301885068628895 ) ) ;
#16144 = DIRECTION ( 'NONE',  ( 0.2490110332224869105, 8.271275069592406292E-16, -0.9685006480810787188 ) ) ;
#16145 = DIRECTION ( 'NONE',  ( 0.000000000000000000, -1.000000000000000000, 0.000000000000000000 ) ) ;
#16146 = CARTESIAN_POINT ( 'NONE',  ( 3.519663612133736130, 13.19443745317615324, 8.148135684914707966 ) ) ;
#16147 = EDGE_LOOP ( 'NONE', ( #7528, #9573, #21316, #2183 ) ) ;
#16148 = DIRECTION ( 'NONE',  ( 0.8558687090795834562, 0.000000000000000000, -0.5171931484643310650 ) ) ;
#16149 = CARTESIAN_POINT ( 'NONE',  ( 12.88040283537677588, -5.959792500000001603, -0.09070320285213756550 ) ) ;
#16150 = CARTESIAN_POINT ( 'NONE',  ( 8.781357490942916399, -7.547927499999999235, -18.85455479843708559 ) ) ;
#16151 = DIRECTION ( 'NONE',  ( 0.05085730733808393328, 0.000000000000000000, -0.9987059298363656357 ) ) ;
#16152 = CYLINDRICAL_SURFACE ( 'NONE', #11621, 1.190625000000000711 ) ;
#16153 = ORIENTED_EDGE ( 'NONE', *, *, #9625, .F. ) ;
#16154 = ORIENTED_EDGE ( 'NONE', *, *, #9761, .T. ) ;
#16155 = CARTESIAN_POINT ( 'NONE',  ( 7.100511544796050956, 14.62096091062142023, -1.910049678553054076 ) ) ;
#16156 = AXIS2_PLACEMENT_3D ( 'NONE', #19934, #11110, #21480 ) ;
#16158 = CARTESIAN_POINT ( 'NONE',  ( 1.581041518826207248, 36.51313500000000545, -20.30277549736237575 ) ) ;
#16157 = FACE_BOUND ( 'NONE', #18237, .T. ) ;
#16159 = CARTESIAN_POINT ( 'NONE',  ( 11.45688759763531017, 19.74712408279570397, -3.340234307731413832 ) ) ;
#16160 = ORIENTED_EDGE ( 'NONE', *, *, #8520, .F. ) ;
#16161 = EDGE_CURVE ( 'NONE', #8219, #14025, #1609, .T. ) ;
#16162 = ORIENTED_EDGE ( 'NONE', *, *, #10458, .T. ) ;
#16163 = DIRECTION ( 'NONE',  ( 0.2490110332224850509, 0.000000000000000000, -0.9685006480810792739 ) ) ;
#16164 = CARTESIAN_POINT ( 'NONE',  ( 7.219586368393647646, 15.63079142330355431, -2.842886198857130342 ) ) ;
#16165 = DIRECTION ( 'NONE',  ( 0.000000000000000000, 1.000000000000000000, 0.000000000000000000 ) ) ;
#16166 = CARTESIAN_POINT ( 'NONE',  ( 8.943293099748036212, 18.40455973696678171, 6.765881260930631136 ) ) ;
#16167 = ADVANCED_FACE ( 'NONE', ( #21725 ), #17179, .F. ) ;
#16168 = EDGE_CURVE ( 'NONE', #3169, #10936, #8339, .T. ) ;
#16169 = CARTESIAN_POINT ( 'NONE',  ( 2.339047551884789300, 20.04416362538683316, 6.193340813788498878 ) ) ;
#16170 = FACE_OUTER_BOUND ( 'NONE', #19297, .T. ) ;
#16171 = CARTESIAN_POINT ( 'NONE',  ( 6.585898268469219552, 32.54502000000000095, 4.694966092919240275 ) ) ;
#16172 = VECTOR ( 'NONE', #11347, 1000.000000000000000 ) ;
#16173 = CARTESIAN_POINT ( 'NONE',  ( 6.573394049933097172, 10.79308423060320088, 3.201986252843589842 ) ) ;
#16174 = DIRECTION ( 'NONE',  ( 0.08420877549337302259, 0.000000000000000000, 0.9964481331860212121 ) ) ;
#16175 = CARTESIAN_POINT ( 'NONE',  ( 12.57635667311951622, -1.983739999999999393, 1.354834321244424267 ) ) ;
#16176 = CARTESIAN_POINT ( 'NONE',  ( 1.263792660725098438, 18.94197024501346505, 8.993320458267341166 ) ) ;
#16177 = CARTESIAN_POINT ( 'NONE',  ( 1.645748489547319116, 13.85855418379529702, 8.959199678648232634 ) ) ;
#16178 = LINE ( 'NONE', #1004, #20563 ) ;
#16179 = CARTESIAN_POINT ( 'NONE',  ( 2.541631375165741780, 19.25518317520560174, 0.9982165646741868459 ) ) ;
#16180 = CARTESIAN_POINT ( 'NONE',  ( 53.08681243024872742, 40.07829845791615497, -16.72443647849243575 ) ) ;
#16181 = DIRECTION ( 'NONE',  ( -0.8943161143440100380, 0.000000000000000000, -0.4474356798743612806 ) ) ;
#16182 = CARTESIAN_POINT ( 'NONE',  ( 17.80487650496869279, -7.974366391153033362, -14.46540208612562317 ) ) ;
#16183 = VERTEX_POINT ( 'NONE', #15008 ) ;
#16184 = CARTESIAN_POINT ( 'NONE',  ( -12.30312499999999964, 30.16440499999999858, 8.335010000000000474 ) ) ;
#16185 = CARTESIAN_POINT ( 'NONE',  ( 9.472187362630734242, 11.71793829268833242, -1.348010422977820921 ) ) ;
#16186 = VERTEX_POINT ( 'NONE', #13550 ) ;
#16187 = EDGE_CURVE ( 'NONE', #9371, #13996, #18515, .T. ) ;
#16188 = LINE ( 'NONE', #19369, #7473 ) ;
#16189 = EDGE_CURVE ( 'NONE', #19201, #4193, #10661, .T. ) ;
#16190 = CARTESIAN_POINT ( 'NONE',  ( 11.64281951131889237, 19.29374815207993876, -2.722012555705051184 ) ) ;
#16191 = EDGE_CURVE ( 'NONE', #14525, #12822, #20703, .T. ) ;
#16192 = AXIS2_PLACEMENT_3D ( 'NONE', #19088, #5725, #11136 ) ;
#16193 = CARTESIAN_POINT ( 'NONE',  ( 5.412656472264093743, 13.93293247221977715, -1.594745895433004934 ) ) ;
#16194 = DIRECTION ( 'NONE',  ( 0.08420877549337302259, 0.000000000000000000, 0.9964481331860212121 ) ) ;
#16195 = CARTESIAN_POINT ( 'NONE',  ( 4.492686771805626478, 11.78541955647214046, 3.831345326553988961 ) ) ;
#16196 = ORIENTED_EDGE ( 'NONE', *, *, #6432, .F. ) ;
#16197 = DIRECTION ( 'NONE',  ( 0.000000000000000000, 0.000000000000000000, 1.000000000000000000 ) ) ;
#16198 = DIRECTION ( 'NONE',  ( 0.7421532822901579785, 0.000000000000000000, -0.6702301885068628895 ) ) ;
#16199 = CARTESIAN_POINT ( 'NONE',  ( 42.92377690484065056, 34.52875999999999834, 4.437564921049077071 ) ) ;
#16200 = CARTESIAN_POINT ( 'NONE',  ( 7.927587859631255007, 18.10524492707348898, -2.105417880674745224 ) ) ;
#16201 = CARTESIAN_POINT ( 'NONE',  ( 5.360969217315594726, 15.89262681558415302, 8.016724612055000421 ) ) ;
#16202 = CARTESIAN_POINT ( 'NONE',  ( 21.03437500000000071, 30.56064500000000095, 5.159374999999999822 ) ) ;
#16203 = CARTESIAN_POINT ( 'NONE',  ( 3.546160502010647253, 11.97425653754774189, 6.753784413642313744 ) ) ;
#16204 = LINE ( 'NONE', #12886, #18809 ) ;
#16205 = CARTESIAN_POINT ( 'NONE',  ( 36.73521423675246922, 34.52875999999999834, 2.413462327205186497 ) ) ;
#16206 = CARTESIAN_POINT ( 'NONE',  ( 6.016625000000000334, 30.56064500000000095, 2.794000000000000039 ) ) ;
#16207 = CARTESIAN_POINT ( 'NONE',  ( -16.14706788831979978, -3.968114999999999615, -25.97380585690919830 ) ) ;
#16208 = CARTESIAN_POINT ( 'NONE',  ( 26.59062499999999929, 5.953125000000000000, 8.731249999999999289 ) ) ;
#16209 = VERTEX_POINT ( 'NONE', #5794 ) ;
#16210 = FACE_OUTER_BOUND ( 'NONE', #21842, .T. ) ;
#16211 = DIRECTION ( 'NONE',  ( 0.000000000000000000, -1.000000000000000000, 0.000000000000000000 ) ) ;
#16212 = VERTEX_POINT ( 'NONE', #5558 ) ;
#16213 = EDGE_CURVE ( 'NONE', #18152, #12400, #7935, .T. ) ;
#16214 = CARTESIAN_POINT ( 'NONE',  ( 10.98450716361348611, 21.21059770410760947, 1.107460585341796033 ) ) ;
#16215 = DIRECTION ( 'NONE',  ( 0.7421532822901579785, 0.000000000000000000, -0.6702301885068628895 ) ) ;
#16216 = CARTESIAN_POINT ( 'NONE',  ( 1.474443682498560948, 15.66970848929637228, 8.798798342679392093 ) ) ;
#16217 = CARTESIAN_POINT ( 'NONE',  ( 10.49358939520456779, -3.807072909132312777, -15.50232714196991779 ) ) ;
#16219 = LINE ( 'NONE', #12460, #3232 ) ;
#16218 = CARTESIAN_POINT ( 'NONE',  ( 0.8556435366884832527, 20.72409300549792022, 3.542841960764134601 ) ) ;
#16220 = ORIENTED_EDGE ( 'NONE', *, *, #14384, .F. ) ;
#16221 = CARTESIAN_POINT ( 'NONE',  ( 31.05388211198297554, 32.54502000000000095, -15.23127950648024331 ) ) ;
#16222 = DIRECTION ( 'NONE',  ( 0.2672484743474500268, 0.000000000000000000, 0.9636276526537417286 ) ) ;
#16223 = AXIS2_PLACEMENT_3D ( 'NONE', #1694, #3474, #7121 ) ;
#16224 = ORIENTED_EDGE ( 'NONE', *, *, #18333, .F. ) ;
#16225 = CARTESIAN_POINT ( 'NONE',  ( 19.76774214424137099, -0.5915200861490187423, -14.90326874178355254 ) ) ;
#16226 = CARTESIAN_POINT ( 'NONE',  ( 20.16764906325613893, -0.5540476120351953693, -16.10433982750742743 ) ) ;
#16227 = ORIENTED_EDGE ( 'NONE', *, *, #19747, .T. ) ;
#16228 = CARTESIAN_POINT ( 'NONE',  ( 9.307353458992574602, 13.73189003748300685, -2.234787557808452174 ) ) ;
#16229 = CARTESIAN_POINT ( 'NONE',  ( 9.397344280094475977, 11.74680749646248223, -1.572083189369575251 ) ) ;
#16230 = DIRECTION ( 'NONE',  ( 0.000000000000000000, -1.000000000000000000, 0.000000000000000000 ) ) ;
#16231 = AXIS2_PLACEMENT_3D ( 'NONE', #12027, #5266, #13811 ) ;
#16232 = EDGE_LOOP ( 'NONE', ( #13381, #11022, #13489, #11455 ) ) ;
#16233 = DIRECTION ( 'NONE',  ( -0.000000000000000000, -1.000000000000000000, 0.000000000000000000 ) ) ;
#16234 = PLANE ( 'NONE',  #13001 ) ;
#16235 = ORIENTED_EDGE ( 'NONE', *, *, #6519, .F. ) ;
#16236 = ORIENTED_EDGE ( 'NONE', *, *, #1460, .T. ) ;
#16237 = ADVANCED_FACE ( 'NONE', ( #7241 ), #2252, .F. ) ;
#16238 = AXIS2_PLACEMENT_3D ( 'NONE', #17194, #17305, #12229 ) ;
#16239 = CARTESIAN_POINT ( 'NONE',  ( 13.95773855287893461, 2.289327961384433063, -16.02183746796031372 ) ) ;
#16241 = CARTESIAN_POINT ( 'NONE',  ( 32.52436584422698473, 32.54502000000000095, 1.884807767196291284 ) ) ;
#16240 = CARTESIAN_POINT ( 'NONE',  ( 0.6936882041921323960, 20.32439072914841915, 1.798629773014991162 ) ) ;
#16242 = VERTEX_POINT ( 'NONE', #17621 ) ;
#16243 = CARTESIAN_POINT ( 'NONE',  ( 3.513372137076729906, 15.46707393753248816, -1.345952314047888843 ) ) ;
#16244 = CIRCLE ( 'NONE', #19035, 0.5079999999999965654 ) ;
#16245 = ORIENTED_EDGE ( 'NONE', *, *, #21811, .F. ) ;
#16246 = ORIENTED_EDGE ( 'NONE', *, *, #5082, .F. ) ;
#16247 = ORIENTED_EDGE ( 'NONE', *, *, #2025, .T. ) ;
#16248 = CARTESIAN_POINT ( 'NONE',  ( 2.745171094293236802, 12.05874077879421158, 4.659437464387258920 ) ) ;
#16249 = AXIS2_PLACEMENT_3D ( 'NONE', #6341, #14999, #18792 ) ;
#16250 = FACE_OUTER_BOUND ( 'NONE', #11154, .T. ) ;
#16251 = CIRCLE ( 'NONE', #21879, 0.5079999999999984528 ) ;
#16252 = DIRECTION ( 'NONE',  ( 0.08420877549337300871, 0.000000000000000000, 0.9964481331860212121 ) ) ;
#16253 = CYLINDRICAL_SURFACE ( 'NONE', #1213, 9.524999999999996803 ) ;
#16254 = DIRECTION ( 'NONE',  ( 0.000000000000000000, 1.000000000000000000, 0.000000000000000000 ) ) ;
#16255 = CARTESIAN_POINT ( 'NONE',  ( 3.650123795476809985, 14.95939606358802365, 9.021213235581008405 ) ) ;
#16256 = ORIENTED_EDGE ( 'NONE', *, *, #18456, .T. ) ;
#16257 = DIRECTION ( 'NONE',  ( 0.000000000000000000, -1.000000000000000000, 0.000000000000000000 ) ) ;
#16258 = LINE ( 'NONE', #6280, #10295 ) ;
#16259 = DIRECTION ( 'NONE',  ( 0.3850029901312932989, 0.000000000000000000, -0.9229153252546862252 ) ) ;
#16260 = CARTESIAN_POINT ( 'NONE',  ( 42.94469661997857912, 32.54502000000000095, -18.48251861828712705 ) ) ;
#16261 = DIRECTION ( 'NONE',  ( -0.000000000000000000, -1.000000000000000000, 0.000000000000000000 ) ) ;
#16262 = VERTEX_POINT ( 'NONE', #7444 ) ;
#16263 = VERTEX_POINT ( 'NONE', #12315 ) ;
#16264 = EDGE_CURVE ( 'NONE', #11872, #20613, #17828, .T. ) ;
#16265 = CARTESIAN_POINT ( 'NONE',  ( 10.00659469058676976, 11.17647817907412211, 2.270694458645354796 ) ) ;
#16266 = CIRCLE ( 'NONE', #21191, 0.7950200000000005041 ) ;
#16267 = EDGE_CURVE ( 'NONE', #17189, #8237, #4029, .T. ) ;
#16269 = DIRECTION ( 'NONE',  ( -0.9999999998269335499, -1.860465115957061339E-05, 0.000000000000000000 ) ) ;
#16268 = PLANE ( 'NONE',  #15445 ) ;
#16270 = CARTESIAN_POINT ( 'NONE',  ( 10.92231696702098098, 15.18632195086740566, -4.231608765564518926 ) ) ;
#16271 = ORIENTED_EDGE ( 'NONE', *, *, #13709, .T. ) ;
#16272 = ORIENTED_EDGE ( 'NONE', *, *, #4694, .F. ) ;
#16273 = FACE_OUTER_BOUND ( 'NONE', #6369, .T. ) ;
#16274 = CARTESIAN_POINT ( 'NONE',  ( 8.151680067859278012, 20.73185275495596258, -0.8723213122503620243 ) ) ;
#16275 = AXIS2_PLACEMENT_3D ( 'NONE', #19787, #18038, #11183 ) ;
#16276 = CARTESIAN_POINT ( 'NONE',  ( 8.987010725829778224, 18.18998750146314691, 6.856259478869401569 ) ) ;
#16277 = EDGE_CURVE ( 'NONE', #10812, #5142, #11367, .T. ) ;
#16278 = LINE ( 'NONE', #11499, #9672 ) ;
#16279 = DIRECTION ( 'NONE',  ( -0.5087559856598098396, 0.000000000000000000, -0.8609107660235847392 ) ) ;
#16280 = DIRECTION ( 'NONE',  ( -0.9685006480810790519, 0.000000000000000000, -0.2490110332224857170 ) ) ;
#16281 = CARTESIAN_POINT ( 'NONE',  ( 0.7383804360333685590, 11.42036430616624187, 4.749601484146273478 ) ) ;
#16282 = ORIENTED_EDGE ( 'NONE', *, *, #3410, .T. ) ;
#16283 = VECTOR ( 'NONE', #3605, 1000.000000000000000 ) ;
#16284 = CARTESIAN_POINT ( 'NONE',  ( -0.5539956361495408377, 20.04712316396406280, 3.943730590064324026 ) ) ;
#16285 = DIRECTION ( 'NONE',  ( 0.000000000000000000, -1.000000000000000000, 0.000000000000000000 ) ) ;
#16286 = DIRECTION ( 'NONE',  ( 0.9987059298363656357, 0.000000000000000000, 0.05085730733808393328 ) ) ;
#16287 = CARTESIAN_POINT ( 'NONE',  ( 20.74198381141644631, -4.535585304848481769, -13.88224875571499162 ) ) ;
#16288 = AXIS2_PLACEMENT_3D ( 'NONE', #10426, #18815, #20576 ) ;
#16289 = EDGE_LOOP ( 'NONE', ( #6266, #4199, #8692, #8576 ) ) ;
#16290 = LINE ( 'NONE', #17939, #4993 ) ;
#16291 = EDGE_CURVE ( 'NONE', #6123, #13945, #6619, .T. ) ;
#16292 = CARTESIAN_POINT ( 'NONE',  ( 9.107214270684286461, 14.05054535227951185, -3.143078356159366926 ) ) ;
#16293 = ORIENTED_EDGE ( 'NONE', *, *, #1033, .T. ) ;
#16294 = PRESENTATION_LAYER_ASSIGNMENT (  '', '', ( #20 ) ) ;
#16295 = CARTESIAN_POINT ( 'NONE',  ( 13.64200589084435578, 39.28268749999999443, -0.3187768451312169571 ) ) ;
#16296 = CARTESIAN_POINT ( 'NONE',  ( 5.365966479128769784, 15.46734445848809791, -2.079964192967793224 ) ) ;
#16297 = FACE_OUTER_BOUND ( 'NONE', #7287, .T. ) ;
#16298 = CARTESIAN_POINT ( 'NONE',  ( 1.387271843693158591, 17.16051976808181578, 8.849130394416750534 ) ) ;
#16299 = VECTOR ( 'NONE', #2037, 1000.000000000000227 ) ;
#16300 = VERTEX_POINT ( 'NONE', #12436 ) ;
#16301 = CARTESIAN_POINT ( 'NONE',  ( -2.607150795738780058, 32.54502000000000095, 8.731885000000000119 ) ) ;
#16302 = ADVANCED_FACE ( 'NONE', ( #5450 ), #13891, .T. ) ;
#16303 = PLANE ( 'NONE',  #20621 ) ;
#16304 = CIRCLE ( 'NONE', #14552, 3.175000000000000711 ) ;
#16305 = FACE_OUTER_BOUND ( 'NONE', #9797, .T. ) ;
#16306 = CARTESIAN_POINT ( 'NONE',  ( 8.303166099514529108, 19.61749303057682070, -1.245790386501098190 ) ) ;
#16307 = ADVANCED_FACE ( 'NONE', ( #4132, #19042, #15768, #14105, #8876 ), #14218, .F. ) ;
#16308 = CARTESIAN_POINT ( 'NONE',  ( 3.923284618780132238, 17.33544538521946876, -1.455743775410417440 ) ) ;
#16309 = EDGE_CURVE ( 'NONE', #19273, #9683, #3352, .T. ) ;
#16310 = DIRECTION ( 'NONE',  ( 0.000000000000000000, 1.000000000000000000, 0.000000000000000000 ) ) ;
#16311 = CIRCLE ( 'NONE', #6042, 0.3962400000000003142 ) ;
#16312 = CARTESIAN_POINT ( 'NONE',  ( 6.662566001476148081, 11.59927578851775287, 2.759431188061297391 ) ) ;
#16313 = CARTESIAN_POINT ( 'NONE',  ( -19.99570496368815142, 42.13594019876639862, -10.11526441440630286 ) ) ;
#16314 = CARTESIAN_POINT ( 'NONE',  ( 21.15636133095030758, -2.013917305199845131, -15.09882835708281235 ) ) ;
#16315 = DIRECTION ( 'NONE',  ( 1.000000000000000000, 0.000000000000000000, 0.000000000000000000 ) ) ;
#16316 = ORIENTED_EDGE ( 'NONE', *, *, #12926, .F. ) ;
#16317 = CARTESIAN_POINT ( 'NONE',  ( 30.74535937054756829, -95.96551800000000298, -3.684081112461307317 ) ) ;
#16318 = CARTESIAN_POINT ( 'NONE',  ( 12.13621795668766445, 34.52875999999999834, 4.225309685850866082 ) ) ;
#16319 = ORIENTED_EDGE ( 'NONE', *, *, #3132, .F. ) ;
#16320 = CARTESIAN_POINT ( 'NONE',  ( 11.06533559283524148, 21.23783741712729523, 1.325821793394421411 ) ) ;
#16321 = FACE_OUTER_BOUND ( 'NONE', #14892, .T. ) ;
#16322 = CARTESIAN_POINT ( 'NONE',  ( 20.27068864692651573, -0.3073929331726920067, -14.91500286423835675 ) ) ;
#16323 = CARTESIAN_POINT ( 'NONE',  ( 54.36523883999320361, 0.000000000000000000, -30.28170612544299800 ) ) ;
#16324 = ORIENTED_EDGE ( 'NONE', *, *, #18198, .T. ) ;
#16325 = DIRECTION ( 'NONE',  ( 0.2490110332224850231, 0.000000000000000000, -0.9685006480810791629 ) ) ;
#16326 = LINE ( 'NONE', #15540, #1013 ) ;
#16327 = AXIS2_PLACEMENT_3D ( 'NONE', #3541, #18784, #10277 ) ;
#16328 = VECTOR ( 'NONE', #11414, 1000.000000000000000 ) ;
#16329 = ORIENTED_EDGE ( 'NONE', *, *, #11902, .F. ) ;
#16330 = CARTESIAN_POINT ( 'NONE',  ( 19.88373355471720316, -0.8065084006328289146, -14.86228188206940892 ) ) ;
#16331 = AXIS2_PLACEMENT_3D ( 'NONE', #13698, #12025, #3628 ) ;
#16332 = CARTESIAN_POINT ( 'NONE',  ( 17.10804421600703051, 1.342424645466655964, -15.60784635835710255 ) ) ;
#16333 = ORIENTED_EDGE ( 'NONE', *, *, #15870, .T. ) ;
#16334 = B_SPLINE_CURVE_WITH_KNOTS ( 'NONE', 3,
 ( #19113, #6251, #19224, #1177, #19627, #15936, #1059, #14794, #7805, #14581, #11232, #6150, #12918, #13025, #18207, #19846, #5627, #17981, #7918, #21398, #4603, #18096, #2955, #9681, #21505, #9885, #5137, #19955, #16654, #8125, #3597, #4827, #3279, #8446, #10011, #15015, #1497, #8345, #11888, #5235, #3157, #15218, #20371, #6689, #18728, #16765, #11562, #21732, #1604, #18299, #1817, #21621, #11784, #8242, #18616, #13559, #163, #4921, #15118, #16550, #6481, #18404, #5033, #1707, #13245, #6586, #10220, #20265, #13348, #21834, #3483, #16861, #18517, #8559, #6908, #13448, #20052, #11668, #13669, #3383, #20158, #10114, #47, #6801, #12325, #5803, #17420, #14230, #8770, #7135, #2374, #15882, #15551, #1925, #7456, #15442, #13905, #5687, #19052, #270, #17186, #20601, #603, #12559, #707, #20947, #19282, #18840, #8669, #10672, #10339, #12448, #4036, #2145, #12115, #5459, #2261, #9001, #3707, #17081, #15778, #7348, #10449, #13778, #9102, #20482, #12222, #2028, #18943, #10551, #5354, #19173, #3815, #10780, #17297, #15670, #8889, #14115, #20818, #17527, #3193, #8274, #10145, #5167, #196, #5492, #5267, #15701, #11820, #7278, #3413, #6938, #2062, #13597, #8595, #6837, #86, #416, #7046, #16891, #11918, #20632, #7170, #17220, #20298, #13934, #18549, #20518, #20199, #3850, #15579, #1741, #10478, #10372, #5386, #13812, #13701, #17118, #15477, #8480, #8698, #529, #20401, #12149, #5069, #18874, #2181, #10588, #10253, #8923, #12028, #1960, #15259, #3517, #303, #18647, #17000, #17333, #12252, #1854, #18761, #15373, #3631, #3743, #8803 ),
 .UNSPECIFIED., .F., .F.,
 ( 4, 3, 3, 3, 3, 3, 3, 3, 3, 3, 3, 3, 3, 3, 3, 3, 3, 3, 3, 3, 3, 3, 3, 3, 3, 3, 3, 3, 3, 3, 3, 3, 3, 3, 3, 3, 3, 3, 3, 3, 3, 3, 3, 3, 3, 3, 3, 3, 3, 3, 3, 3, 3, 3, 3, 3, 3, 3, 3, 3, 3, 3, 3, 3, 3, 3, 3, 3, 4 ),
 ( 3.118384633268010597E-11, 0.01886792455889550052, 0.03773584908660710530, 0.04500012977624090471, 0.05660377361432869514, 0.07547169814204039706, 0.09433962266975200184, 0.1099999085797309928, 0.1132075471974540032, 0.1320754717251650112, 0.1509433962528770046, 0.1698113207805879987, 0.1750001347259370066, 0.1886792453082999921, 0.2075471698360119854, 0.2264150943637230073, 0.2399998702385330029, 0.2452830188914350007, 0.2641509434191470218, 0.2830188679468579882, 0.3018867924745700093, 0.3050000920636670165, 0.3207547170022810312, 0.3396226415299929968, 0.3584905660577050179, 0.3699999077873000197, 0.3773584905854159843, 0.3962264151131280054, 0.4150943396408399710, 0.4339622641685509929, 0.4350000229552469788, 0.4528301886962630141, 0.4716981132239739805, 0.4905660377516860016, 0.5000000065312421027, 0.5094339622794979983, 0.5283018868072090202, 0.5471698113349209303, 0.5649999901081249609, 0.5660377358626329514, 0.5849056603903439733, 0.6037735849180559944, 0.6226415094457670163, 0.6300001052753160247, 0.6415094339734789264, 0.6603773585011909475, 0.6792452830289019694, 0.6949999209998329874, 0.6981132075566139905, 0.7169811320843260116, 0.7358490566120369225, 0.7547169811397489436, 0.7600001428246599966, 0.7735849056674599655, 0.7924528301951719866, 0.8113207547228840077, 0.8249998783372239908, 0.8301886792505950297, 0.8490566037783069397, 0.8679245283060189609, 0.8867924528337299828, 0.8900001044837360098, 0.9056603773614420039, 0.9245283018891530258, 0.9433962264168649359, 0.9549998832863340059, 0.9622641509445769570, 0.9811320754722879789, 1.000000000000000000 ),
 .UNSPECIFIED. ) ;
#16335 = CARTESIAN_POINT ( 'NONE',  ( 11.97860041647407314, 11.13144644120788307, 0.7672358936978520561 ) ) ;
#16336 = EDGE_CURVE ( 'NONE', #20642, #10436, #3692, .T. ) ;
#16337 = CARTESIAN_POINT ( 'NONE',  ( 10.29335322697429511, 10.45400687491624225, 2.209017800539377241 ) ) ;
#16338 = AXIS2_PLACEMENT_3D ( 'NONE', #520, #10697, #4167 ) ;
#16339 = CARTESIAN_POINT ( 'NONE',  ( 45.99559936598748777, 0.000000000000000000, 5.449572532947073000 ) ) ;
#16340 = ORIENTED_EDGE ( 'NONE', *, *, #6650, .F. ) ;
#16341 = CARTESIAN_POINT ( 'NONE',  ( 30.78626241496060700, -5.959792500000001603, -2.552201779827368622 ) ) ;
#16342 = CARTESIAN_POINT ( 'NONE',  ( 12.11879977990919421, 19.43893749999999798, 0.1373704394269426865 ) ) ;
#16343 = VERTEX_POINT ( 'NONE', #10872 ) ;
#16344 = ORIENTED_EDGE ( 'NONE', *, *, #316, .T. ) ;
#16345 = CARTESIAN_POINT ( 'NONE',  ( 54.36523883999320361, 74.97070807199999365, -30.28170612544299800 ) ) ;
#16346 = AXIS2_PLACEMENT_3D ( 'NONE', #10987, #20599, #5457 ) ;
#16348 = CARTESIAN_POINT ( 'NONE',  ( 47.80475250345343596, 40.07865999999999929, -11.91473563638196786 ) ) ;
#16347 = CARTESIAN_POINT ( 'NONE',  ( 4.894910957408831642, 21.42306324396562189, 2.018202348579825056 ) ) ;
#16349 = ORIENTED_EDGE ( 'NONE', *, *, #21331, .T. ) ;
#16350 = CARTESIAN_POINT ( 'NONE',  ( 4.360118323002954988, 20.34695651380200587, 0.3338233916395515477 ) ) ;
#16351 = VERTEX_POINT ( 'NONE', #2474 ) ;
#16352 = ORIENTED_EDGE ( 'NONE', *, *, #12494, .T. ) ;
#16353 = CARTESIAN_POINT ( 'NONE',  ( 0.8183488901082509592, 12.22193901380214065, 5.111763293916161466 ) ) ;
#16354 = ORIENTED_EDGE ( 'NONE', *, *, #18578, .T. ) ;
#16355 = ADVANCED_FACE ( 'NONE', ( #15985 ), #18935, .F. ) ;
#16356 = CARTESIAN_POINT ( 'NONE',  ( 4.111172719939895970, 12.39521241338711199, 1.660306762232565791 ) ) ;
#16357 = AXIS2_PLACEMENT_3D ( 'NONE', #14197, #796, #15521 ) ;
#16358 = DIRECTION ( 'NONE',  ( -0.5087559856598088404, 0.000000000000000000, -0.8609107660235851833 ) ) ;
#16359 = CARTESIAN_POINT ( 'NONE',  ( 29.98909767165928386, 29.75768749999999940, -5.214162619065493054 ) ) ;
#16360 = DIRECTION ( 'NONE',  ( -0.9964481331860213231, 0.000000000000000000, 0.08420877549337293932 ) ) ;
#16361 = DIRECTION ( 'NONE',  ( -0.2490110332224850509, 0.000000000000000000, 0.9685006480810792739 ) ) ;
#16362 = CARTESIAN_POINT ( 'NONE',  ( 3.294987831897750574, 12.14111609449092555, 7.060071635313232008 ) ) ;
#16363 = ORIENTED_EDGE ( 'NONE', *, *, #16309, .F. ) ;
#16364 = DIRECTION ( 'NONE',  ( -0.1727088819286940469, 0.000000000000000000, 0.9849729144006653669 ) ) ;
#16365 = DIRECTION ( 'NONE',  ( 0.000000000000000000, -1.000000000000000000, 0.000000000000000000 ) ) ;
#16366 = CARTESIAN_POINT ( 'NONE',  ( 29.22749461619170219, 30.50833916023545811, -4.986088976786413163 ) ) ;
#16367 =( LENGTH_UNIT ( ) NAMED_UNIT ( * ) SI_UNIT ( .MILLI., .METRE. ) );
#16368 = CARTESIAN_POINT ( 'NONE',  ( 53.31385684162800942, 37.72911631579626146, -16.46698546251109008 ) ) ;
#16369 = VECTOR ( 'NONE', #8972, 1000.000000000000227 ) ;
#16370 = EDGE_LOOP ( 'NONE', ( #21623, #15076 ) ) ;
#16371 = ORIENTED_EDGE ( 'NONE', *, *, #16728, .F. ) ;
#16372 = CARTESIAN_POINT ( 'NONE',  ( 6.538910913721166729, 11.94621801824261986, 4.894387607941162344 ) ) ;
#16374 = DIRECTION ( 'NONE',  ( 0.000000000000000000, 1.000000000000000000, 0.000000000000000000 ) ) ;
#16373 = CARTESIAN_POINT ( 'NONE',  ( -21.34815828341188393, 32.54247999999999763, 0.8078590638549643099 ) ) ;
#16375 = CARTESIAN_POINT ( 'NONE',  ( 12.41424834072428141, 21.83950410014850974, -0.7887902040342423815 ) ) ;
#16376 = EDGE_LOOP ( 'NONE', ( #15581, #18656, #5139, #10998 ) ) ;
#16377 = ORIENTED_EDGE ( 'NONE', *, *, #7611, .F. ) ;
#16378 = CARTESIAN_POINT ( 'NONE',  ( 55.56250000000000000, 1.984375000000000000, -10.31874999999999964 ) ) ;
#16379 = CIRCLE ( 'NONE', #4376, 9.524999999999996803 ) ;
#16380 = CARTESIAN_POINT ( 'NONE',  ( 9.125410677652650904, 17.38129722174117120, 7.116283853237153956 ) ) ;
#16381 = CARTESIAN_POINT ( 'NONE',  ( 3.342783359414524202, 16.78689288444595107, 8.424322633587635778 ) ) ;
#16382 = EDGE_CURVE ( 'NONE', #12990, #10772, #12214, .T. ) ;
#16383 = CYLINDRICAL_SURFACE ( 'NONE', #10929, 5.158739999999998105 ) ;
#16384 = CARTESIAN_POINT ( 'NONE',  ( 13.39756118469465029, 22.16307784260286340, 1.948616576935187750 ) ) ;
#16385 = CARTESIAN_POINT ( 'NONE',  ( 66.87634738983680904, 30.56064500000000095, 3.497859541731999755 ) ) ;
#16386 = CARTESIAN_POINT ( 'NONE',  ( 9.828862065001116477, 36.51313500000000545, -16.12522240043857025 ) ) ;
#16387 = CARTESIAN_POINT ( 'NONE',  ( 4.959019311868959612, 21.41828792979770313, 2.000495739218702607 ) ) ;
#16388 = CARTESIAN_POINT ( 'NONE',  ( 1.696681809872754076, 14.67257190654929566, 9.334167604556698805 ) ) ;
#16389 = CARTESIAN_POINT ( 'NONE',  ( 9.907371917564091746, 36.51313500000000545, -13.23786778167655243 ) ) ;
#16390 = ORIENTED_EDGE ( 'NONE', *, *, #16436, .F. ) ;
#16391 = CARTESIAN_POINT ( 'NONE',  ( 7.273569272673938713, 16.58792154420486042, 7.724425322274861117 ) ) ;
#16392 = VECTOR ( 'NONE', #17266, 1000.000000000000000 ) ;
#16393 = DIRECTION ( 'NONE',  ( 0.000000000000000000, 0.000000000000000000, 1.000000000000000000 ) ) ;
#16394 = DIRECTION ( 'NONE',  ( 0.2868778675745004558, 0.000000000000000000, 0.9579671649362035968 ) ) ;
#16395 = CARTESIAN_POINT ( 'NONE',  ( 20.82425928449433528, -4.245348575377335898, -13.87212089903126078 ) ) ;
#16396 = CARTESIAN_POINT ( 'NONE',  ( 61.56621290189396944, 32.54502000000000095, -0.7977859469341201937 ) ) ;
#16397 = VERTEX_POINT ( 'NONE', #13207 ) ;
#16398 = CARTESIAN_POINT ( 'NONE',  ( 32.10373694497760511, -6.356984999999999886, -3.785462747693984831 ) ) ;
#16399 = CARTESIAN_POINT ( 'NONE',  ( 5.363510341419825522, 17.41197255053186055, -2.152950441668251891 ) ) ;
#16400 = CARTESIAN_POINT ( 'NONE',  ( 10.57816040564219229, 21.72525362062316390, -0.03273866274248853070 ) ) ;
#16401 = ORIENTED_EDGE ( 'NONE', *, *, #21481, .T. ) ;
#16402 = VECTOR ( 'NONE', #15820, 1000.000000000000000 ) ;
#16403 = DIRECTION ( 'NONE',  ( -0.000000000000000000, -1.000000000000000000, 0.000000000000000000 ) ) ;
#16404 = CARTESIAN_POINT ( 'NONE',  ( 7.679949084132842607, 21.66123601093154960, 3.598503736773588368 ) ) ;
#16405 = DIRECTION ( 'NONE',  ( 0.000000000000000000, 1.000000000000000000, 0.000000000000000000 ) ) ;
#16406 = CARTESIAN_POINT ( 'NONE',  ( 0.2332795718711392907, 20.17752205389220066, 6.179227157311926177 ) ) ;
#16407 = ADVANCED_FACE ( 'NONE', ( #1344 ), #17849, .F. ) ;
#16408 = FILL_AREA_STYLE_COLOUR ( '', #20821 ) ;
#16409 =( REPRESENTATION_RELATIONSHIP ('NONE','NONE', #15554, #13411 ) REPRESENTATION_RELATIONSHIP_WITH_TRANSFORMATION ( #4028 )SHAPE_REPRESENTATION_RELATIONSHIP( ) );
#16410 = DIRECTION ( 'NONE',  ( 0.000000000000000000, -1.000000000000000000, -0.000000000000000000 ) ) ;
#16411 = VECTOR ( 'NONE', #1915, 1000.000000000000000 ) ;
#16412 = EDGE_CURVE ( 'NONE', #7070, #21386, #1911, .T. ) ;
#16413 = EDGE_CURVE ( 'NONE', #4759, #7865, #17104, .T. ) ;
#16414 = CARTESIAN_POINT ( 'NONE',  ( 11.56370448131011841, 15.74068497743424189, 6.880329954670749260 ) ) ;
#16415 = ADVANCED_FACE ( 'NONE', ( #19489 ), #21580, .T. ) ;
#16416 = CARTESIAN_POINT ( 'NONE',  ( 4.938346711425525726, 18.70539829994152115, 7.357799927494061087 ) ) ;
#16417 = AXIS2_PLACEMENT_3D ( 'NONE', #18272, #4893, #14545 ) ;
#16418 = CARTESIAN_POINT ( 'NONE',  ( -22.75431282566211522, -8.248365470396340271, -25.41543459098148716 ) ) ;
#16419 = CARTESIAN_POINT ( 'NONE',  ( -0.1301685750265853259, 15.59583246595391692, -0.03297570318400730449 ) ) ;
#16420 = DIRECTION ( 'NONE',  ( 0.000000000000000000, 1.000000000000000000, 0.000000000000000000 ) ) ;
#16421 = CARTESIAN_POINT ( 'NONE',  ( 61.03378281434940078, 0.000000000000000000, -11.91737544536021431 ) ) ;
#16422 = DIRECTION ( 'NONE',  ( 0.7421532822901579785, 0.000000000000000000, -0.6702301885068628895 ) ) ;
#16423 = DIRECTION ( 'NONE',  ( -0.4128958666089269647, 0.5884034904305883718, 0.6951966166390366464 ) ) ;
#16424 = DIRECTION ( 'NONE',  ( 0.000000000000000000, 1.000000000000000000, 0.000000000000000000 ) ) ;
#16425 = VERTEX_POINT ( 'NONE', #2799 ) ;
#16426 = CARTESIAN_POINT ( 'NONE',  ( 29.19635173153840313, 0.000000000000000000, -6.218966092919240296 ) ) ;
#16427 = CIRCLE ( 'NONE', #8985, 0.5080000000000022276 ) ;
#16428 = DIRECTION ( 'NONE',  ( 0.6702301885068638887, 0.000000000000000000, 0.7421532822901570903 ) ) ;
#16429 = ORIENTED_EDGE ( 'NONE', *, *, #13437, .F. ) ;
#16430 = CARTESIAN_POINT ( 'NONE',  ( 10.83382871988236928, 21.12904306104314855, 0.7014701641843944513 ) ) ;
#16431 = CARTESIAN_POINT ( 'NONE',  ( 14.43917063414567536, -6.754812500000002551, 2.343183994106907697 ) ) ;
#16432 = DIRECTION ( 'NONE',  ( 0.000000000000000000, -1.000000000000000000, 0.000000000000000000 ) ) ;
#16433 = CARTESIAN_POINT ( 'NONE',  ( 19.40057331552889153, -5.839280184494942461, -15.41429742563731864 ) ) ;
#16434 = DIRECTION ( 'NONE',  ( -0.7421532822901579785, 0.000000000000000000, 0.6702301885068630005 ) ) ;
#16435 = ORIENTED_EDGE ( 'NONE', *, *, #6271, .F. ) ;
#16436 = EDGE_CURVE ( 'NONE', #13360, #14322, #14669, .T. ) ;
#16437 = AXIS2_PLACEMENT_3D ( 'NONE', #4627, #11046, #19755 ) ;
#16438 = DIRECTION ( 'NONE',  ( 0.000000000000000000, 1.000000000000000000, 0.000000000000000000 ) ) ;
#16439 = CARTESIAN_POINT ( 'NONE',  ( 3.752833204253988697, 16.02103694708570814, -0.6544082234691355193 ) ) ;
#16440 = ORIENTED_EDGE ( 'NONE', *, *, #18429, .F. ) ;
#16441 = CARTESIAN_POINT ( 'NONE',  ( 19.55894973361720091, -0.1923335449227899507, -14.98190768515691751 ) ) ;
#16442 = CARTESIAN_POINT ( 'NONE',  ( 0.2870103912946987412, 17.92877166684071710, 1.083135389032180873 ) ) ;
#16443 = CARTESIAN_POINT ( 'NONE',  ( 20.83211096346473568, -2.693633402772701579, -14.60905691900277148 ) ) ;
#16444 = ORIENTED_EDGE ( 'NONE', *, *, #13736, .F. ) ;
#16445 = CARTESIAN_POINT ( 'NONE',  ( 10.65847098557893347, 21.11843953786754113, 0.3043021127257425906 ) ) ;
#16446 = EDGE_CURVE ( 'NONE', #12265, #5334, #17951, .T. ) ;
#16447 = CARTESIAN_POINT ( 'NONE',  ( 29.37324403177899868, 30.56064500000000095, -10.70578951775076071 ) ) ;
#16448 = CARTESIAN_POINT ( 'NONE',  ( 10.41141284089941799, 21.01241846032922211, 5.365001480791137922 ) ) ;
#16449 = VECTOR ( 'NONE', #16882, 1000.000000000000000 ) ;
#16450 = ORIENTED_EDGE ( 'NONE', *, *, #8047, .F. ) ;
#16451 = CARTESIAN_POINT ( 'NONE',  ( 3.360635606688116894, -1.983739999999999393, -20.45316710734507026 ) ) ;
#16452 = CARTESIAN_POINT ( 'NONE',  ( 29.64606458365116737, 39.28205249999999893, -15.53894806404596096 ) ) ;
#16453 = ORIENTED_EDGE ( 'NONE', *, *, #1816, .T. ) ;
#16454 = EDGE_LOOP ( 'NONE', ( #15836, #7047, #13577, #20705 ) ) ;
#16455 = CARTESIAN_POINT ( 'NONE',  ( 11.62409918280433985, -6.986177739752845284, -15.77901157387964126 ) ) ;
#16457 = CARTESIAN_POINT ( 'NONE',  ( 2.063750000000000195, 30.56064500000000095, 8.335010000000000474 ) ) ;
#16456 = CARTESIAN_POINT ( 'NONE',  ( 7.343712728639111731, 12.97967409473248246, 7.433702222329153564 ) ) ;
#16458 = ORIENTED_EDGE ( 'NONE', *, *, #14023, .F. ) ;
#16459 = CARTESIAN_POINT ( 'NONE',  ( 3.654533980080661326, 17.51885244241539041, -1.309317591557538574 ) ) ;
#16460 = EDGE_CURVE ( 'NONE', #16563, #17300, #7575, .T. ) ;
#16461 = ORIENTED_EDGE ( 'NONE', *, *, #11755, .T. ) ;
#16462 = EDGE_CURVE ( 'NONE', #16972, #14185, #19599, .T. ) ;
#16463 = ORIENTED_EDGE ( 'NONE', *, *, #4535, .F. ) ;
#16464 = CIRCLE ( 'NONE', #13283, 0.3962399999999988154 ) ;
#16465 = EDGE_LOOP ( 'NONE', ( #1641, #3776, #8786, #4532 ) ) ;
#16466 = CARTESIAN_POINT ( 'NONE',  ( 4.192958223415248931, 12.21630804426136230, 2.039899256093704594 ) ) ;
#16467 = LINE ( 'NONE', #8041, #9586 ) ;
#16468 = CYLINDRICAL_SURFACE ( 'NONE', #19218, 1.190625000000000711 ) ;
#16469 = CARTESIAN_POINT ( 'NONE',  ( -24.20935654380574320, -8.889364999999999739, -25.29247038871795894 ) ) ;
#16470 = CARTESIAN_POINT ( 'NONE',  ( 27.93207353965470574, 0.000000000000000000, -8.388685343514779902 ) ) ;
#16471 = CARTESIAN_POINT ( 'NONE',  ( 3.491312425488612980, 13.00100667128629262, 7.999424012500742975 ) ) ;
#16472 = ORIENTED_EDGE ( 'NONE', *, *, #19795, .T. ) ;
#16473 = DIRECTION ( 'NONE',  ( -0.9790635044817342925, 0.000000000000000000, 0.2035550397114870846 ) ) ;
#16474 = DIRECTION ( 'NONE',  ( -0.2490110332224857170, 0.000000000000000000, 0.9685006480810790519 ) ) ;
#16475 = DIRECTION ( 'NONE',  ( 1.000000000000000000, 0.000000000000000000, 0.000000000000000000 ) ) ;
#16476 = CARTESIAN_POINT ( 'NONE',  ( 50.52547294529469468, 38.88803500000000213, -18.64987929725020521 ) ) ;
#16477 = ORIENTED_EDGE ( 'NONE', *, *, #16462, .F. ) ;
#16478 = ORIENTED_EDGE ( 'NONE', *, *, #6855, .F. ) ;
#16479 = CARTESIAN_POINT ( 'NONE',  ( 10.81808670305476028, 17.53555608635337393, 6.953175927443941973 ) ) ;
#16480 = CARTESIAN_POINT ( 'NONE',  ( 30.41963056417667488, 0.000000000000000000, -8.653862521447852174 ) ) ;
#16481 = CARTESIAN_POINT ( 'NONE',  ( 11.12006939743884537, 18.08540889854115363, -4.117412775282417670 ) ) ;
#16482 = ORIENTED_EDGE ( 'NONE', *, *, #19213, .T. ) ;
#16483 = ORIENTED_EDGE ( 'NONE', *, *, #15458, .F. ) ;
#16484 = EDGE_CURVE ( 'NONE', #2732, #6731, #21695, .T. ) ;
#16485 = DIRECTION ( 'NONE',  ( 0.000000000000000000, 1.000000000000000000, 0.000000000000000000 ) ) ;
#16486 = CYLINDRICAL_SURFACE ( 'NONE', #21114, 0.7950200000000005041 ) ;
#16487 = CARTESIAN_POINT ( 'NONE',  ( 8.821459635400524135, 12.02303503703761223, 4.606412285287802888 ) ) ;
#16488 = CARTESIAN_POINT ( 'NONE',  ( 13.70619102061564298, 21.99218769696788200, 1.831112504243990413 ) ) ;
#16489 = DIRECTION ( 'NONE',  ( -0.2490110332224850231, 0.000000000000000000, 0.9685006480810791629 ) ) ;
#16490 = CARTESIAN_POINT ( 'NONE',  ( 5.454615826616862506, 17.51021144529294560, 8.784396340176970241 ) ) ;
#16491 = CARTESIAN_POINT ( 'NONE',  ( 1.695370511798163671, 15.71096035366437427, 9.573348142837362573 ) ) ;
#16492 = CARTESIAN_POINT ( 'NONE',  ( 2.520748753591570690, -1.594802499999999013, -24.56335908395234924 ) ) ;
#16493 = VECTOR ( 'NONE', #12613, 1000.000000000000000 ) ;
#16494 = ORIENTED_EDGE ( 'NONE', *, *, #21481, .F. ) ;
#16495 = CARTESIAN_POINT ( 'NONE',  ( 0.1287471594020603571, 14.29405283160754614, 1.226153466862331065 ) ) ;
#16496 = CARTESIAN_POINT ( 'NONE',  ( -17.46249999999999858, -1.587500000000002132, 0.000000000000000000 ) ) ;
#16497 = DIRECTION ( 'NONE',  ( 0.9579671649362032637, 0.000000000000000000, -0.2868778675745010664 ) ) ;
#16498 = CARTESIAN_POINT ( 'NONE',  ( 17.13928781705268989, -8.220053430339435252, -14.61006923465378904 ) ) ;
#16499 = VERTEX_POINT ( 'NONE', #12767 ) ;
#16500 = DIRECTION ( 'NONE',  ( 0.000000000000000000, 1.000000000000000000, 0.000000000000000000 ) ) ;
#16501 = CARTESIAN_POINT ( 'NONE',  ( 7.292876639776774361, 12.62524416591024057, -1.628278476874152947 ) ) ;
#16502 = CARTESIAN_POINT ( 'NONE',  ( 9.610208719281146728, 19.70821819264820718, -2.605398466078559849 ) ) ;
#16503 = EDGE_LOOP ( 'NONE', ( #7138, #3886, #15379, #14108 ) ) ;
#16504 = EDGE_CURVE ( 'NONE', #9951, #1425, #7987, .T. ) ;
#16505 = CARTESIAN_POINT ( 'NONE',  ( 8.915785587245871113, 19.67583050180649806, 6.892551414178150537 ) ) ;
#16506 = CARTESIAN_POINT ( 'NONE',  ( 28.97711086133420366, 30.56064500000000095, -10.31874999999999964 ) ) ;
#16507 = CARTESIAN_POINT ( 'NONE',  ( 3.158507891489228836, 12.59229297301672190, 6.478546931336934378 ) ) ;
#16508 = PRESENTATION_STYLE_ASSIGNMENT (( #4680 ) ) ;
#16509 = CARTESIAN_POINT ( 'NONE',  ( 6.892929529354196561, 18.75718618419412564, 6.956112666771808506 ) ) ;
#16510 = AXIS2_PLACEMENT_3D ( 'NONE', #2623, #17982, #17776 ) ;
#16511 = CARTESIAN_POINT ( 'NONE',  ( 11.82678039945931481, 36.51313500000000545, -12.74436900065013667 ) ) ;
#16512 = CARTESIAN_POINT ( 'NONE',  ( 53.25483508941461963, -1.983739999999997838, -5.879799058943532941 ) ) ;
#16513 = CARTESIAN_POINT ( 'NONE',  ( 11.32992743752204312, 12.55266643930576187, 5.310610498300123439 ) ) ;
#16514 = DIRECTION ( 'NONE',  ( 0.000000000000000000, 1.000000000000000000, 0.000000000000000000 ) ) ;
#16515 = CARTESIAN_POINT ( 'NONE',  ( 7.847407104022815716, 14.74276822600529258, 8.097202368905350056 ) ) ;
#16516 = DIRECTION ( 'NONE',  ( -0.2490110332224850509, 0.000000000000000000, 0.9685006480810792739 ) ) ;
#16517 = CARTESIAN_POINT ( 'NONE',  ( -160.2647810241784896, 30.56064500000000095, 10.71562489836746046 ) ) ;
#16518 = CARTESIAN_POINT ( 'NONE',  ( -24.20935654380574320, -8.889364999999999739, -25.29247038871795894 ) ) ;
#16519 = CYLINDRICAL_SURFACE ( 'NONE', #1260, 0.3962400000000008138 ) ;
#16520 = EDGE_CURVE ( 'NONE', #7786, #21204, #1024, .T. ) ;
#16521 = DIRECTION ( 'NONE',  ( 0.000000000000000000, 1.000000000000000000, 0.000000000000000000 ) ) ;
#16522 = ADVANCED_FACE ( 'NONE', ( #11198 ), #2586, .T. ) ;
#16523 = FACE_OUTER_BOUND ( 'NONE', #14808, .T. ) ;
#16524 = ORIENTED_EDGE ( 'NONE', *, *, #9775, .F. ) ;
#16525 = FACE_OUTER_BOUND ( 'NONE', #21309, .T. ) ;
#16526 = CARTESIAN_POINT ( 'NONE',  ( 20.50050043015025025, -0.2396794266589334643, -15.37230335780461310 ) ) ;
#16527 = LINE ( 'NONE', #1358, #12611 ) ;
#16528 = ORIENTED_EDGE ( 'NONE', *, *, #18379, .T. ) ;
#16529 = EDGE_CURVE ( 'NONE', #15944, #21849, #14537, .T. ) ;
#16530 = CARTESIAN_POINT ( 'NONE',  ( 13.10365782807650525, 16.69016472798375972, 6.399640439207225917 ) ) ;
#16531 = CARTESIAN_POINT ( 'NONE',  ( 0.05261182704408059324, 9.129395000000000593, 7.316601101023040066 ) ) ;
#16532 = LINE ( 'NONE', #19938, #19518 ) ;
#16533 = EDGE_CURVE ( 'NONE', #1298, #9903, #11520, .T. ) ;
#16534 = CARTESIAN_POINT ( 'NONE',  ( 19.38529025477529899, -5.351634827297560904, -14.03627082355416178 ) ) ;
#16535 = LINE ( 'NONE', #1366, #18744 ) ;
#16536 = VERTEX_POINT ( 'NONE', #21256 ) ;
#16537 = LINE ( 'NONE', #6021, #4290 ) ;
#16538 = CARTESIAN_POINT ( 'NONE',  ( 4.010039403972132988, 18.11389644008795585, -0.3279598888530740886 ) ) ;
#16539 = LINE ( 'NONE', #9668, #6292 ) ;
#16540 = ORIENTED_EDGE ( 'NONE', *, *, #15611, .T. ) ;
#16541 = CARTESIAN_POINT ( 'NONE',  ( 19.40504022072852663, 0.1453320723159260697, -15.03681954599216652 ) ) ;
#16542 = AXIS2_PLACEMENT_3D ( 'NONE', #8518, #6873, #16823 ) ;
#16543 = CARTESIAN_POINT ( 'NONE',  ( 17.61528648211390902, -7.258561849689513679, -14.99581366938190818 ) ) ;
#16544 = ORIENTED_EDGE ( 'NONE', *, *, #8406, .F. ) ;
#16545 = CARTESIAN_POINT ( 'NONE',  ( 7.395190866011299491, 14.64975276093931100, -1.912940321280476752 ) ) ;
#16546 = CARTESIAN_POINT ( 'NONE',  ( -5.863861779363051419, -1.594802499999999013, -34.80955303575778714 ) ) ;
#16547 = CARTESIAN_POINT ( 'NONE',  ( 12.00188337831979801, 21.69121361356170397, 3.968932558729561411 ) ) ;
#16548 = AXIS2_PLACEMENT_3D ( 'NONE', #3047, #8110, #13434 ) ;
#16549 = EDGE_CURVE ( 'NONE', #16977, #1209, #2992, .T. ) ;
#16550 = CARTESIAN_POINT ( 'NONE',  ( 12.88764127389737446, -5.800509336186265408, -16.71032010666468537 ) ) ;
#16551 = DIRECTION ( 'NONE',  ( 0.000000000000000000, 1.000000000000000000, 0.000000000000000000 ) ) ;
#16552 = ORIENTED_EDGE ( 'NONE', *, *, #3097, .F. ) ;
#16553 = CARTESIAN_POINT ( 'NONE',  ( 8.109003715218610964, 19.66538549285581539, -0.8655619987938839577 ) ) ;
#16554 = CARTESIAN_POINT ( 'NONE',  ( 9.856817040269220342, 10.74905493727258232, 0.1947764129590014437 ) ) ;
#16555 = DIRECTION ( 'NONE',  ( -0.9685006480810792739, 0.000000000000000000, -0.2490110332224846346 ) ) ;
#16556 = ORIENTED_EDGE ( 'NONE', *, *, #3350, .T. ) ;
#16557 = ORIENTED_EDGE ( 'NONE', *, *, #15721, .T. ) ;
#16558 = CIRCLE ( 'NONE', #1696, 6.350000000000002309 ) ;
#16559 = CARTESIAN_POINT ( 'NONE',  ( -17.46249999999999858, -0.3962399999999990929, 0.000000000000000000 ) ) ;
#16560 = ADVANCED_FACE ( 'NONE', ( #12880 ), #16303, .F. ) ;
#16562 = CARTESIAN_POINT ( 'NONE',  ( 61.81956123787853130, 32.54502000000000095, -1.238102447480925239 ) ) ;
#16561 = CARTESIAN_POINT ( 'NONE',  ( -0.2589530521705579180, 13.90637430850843081, 0.5894001625122522459 ) ) ;
#16563 = VERTEX_POINT ( 'NONE', #13097 ) ;
#16564 = CARTESIAN_POINT ( 'NONE',  ( 6.263355025072034010, 21.08859062641374038, 5.475190995882099010 ) ) ;
#16565 = VERTEX_POINT ( 'NONE', #19806 ) ;
#16566 = ORIENTED_EDGE ( 'NONE', *, *, #11884, .T. ) ;
#16567 = DIRECTION ( 'NONE',  ( -0.7532174416907914116, 0.000000000000000000, -0.6577716059034314222 ) ) ;
#16568 = VERTEX_POINT ( 'NONE', #11424 ) ;
#16569 = CARTESIAN_POINT ( 'NONE',  ( 9.920056955027456880, 10.74433361426668121, 0.1741698353093955043 ) ) ;
#16570 = CIRCLE ( 'NONE', #4910, 0.5080000000000013394 ) ;
#16571 = B_SPLINE_CURVE_WITH_KNOTS ( 'NONE', 3,
 ( #7587, #17872, #11007, #11120, #19188, #21063, #4158, #2497, #4054, #12464, #7690, #10797, #17766, #5913, #5818, #12573, #9451, #17542 ),
 .UNSPECIFIED., .F., .F.,
 ( 4, 2, 2, 2, 2, 2, 2, 2, 4 ),
 ( 0.000000000000000000, 0.0004692937272967113212, 0.0009385874545934226425, 0.001407881181890133964, 0.001877174909186845285, 0.002346468636483556823, 0.002815762363780267927, 0.003285056091076979032, 0.003754349818373690570 ),
 .UNSPECIFIED. ) ;
#16572 = DIRECTION ( 'NONE',  ( 0.000000000000000000, -1.000000000000000000, -0.000000000000000000 ) ) ;
#16573 = EDGE_CURVE ( 'NONE', #9687, #15542, #18171, .T. ) ;
#16574 = CYLINDRICAL_SURFACE ( 'NONE', #857, 2.381250000000001421 ) ;
#16575 = DIRECTION ( 'NONE',  ( -0.9987059298363657467, 0.000000000000000000, -0.05085730733808409287 ) ) ;
#16576 = CARTESIAN_POINT ( 'NONE',  ( 1.853075885237863929, 17.83409906757449548, -0.4903821156112312396 ) ) ;
#16577 = EDGE_CURVE ( 'NONE', #1966, #10716, #15182, .T. ) ;
#16578 = EDGE_CURVE ( 'NONE', #8349, #9790, #9847, .T. ) ;
#16579 = ORIENTED_EDGE ( 'NONE', *, *, #1543, .F. ) ;
#16580 = CARTESIAN_POINT ( 'NONE',  ( 57.35354854712898742, 37.11476346399999926, -21.22263945788050776 ) ) ;
#16581 = CYLINDRICAL_SURFACE ( 'NONE', #7830, 0.7950199999999993938 ) ;
#16582 = CARTESIAN_POINT ( 'NONE',  ( 23.15492293361681320, 23.80367230640320031, -3.167564836549936480 ) ) ;
#16583 = CARTESIAN_POINT ( 'NONE',  ( 53.84899360340892827, 39.04632977872977051, -15.76908876899390322 ) ) ;
#16584 = ORIENTED_EDGE ( 'NONE', *, *, #8598, .T. ) ;
#16585 = EDGE_LOOP ( 'NONE', ( #13279, #15446, #6711, #18932, #7446 ) ) ;
#16586 = CARTESIAN_POINT ( 'NONE',  ( 12.61172719285503341, 18.50160361240584095, 6.235549524936597976 ) ) ;
#16587 = LINE ( 'NONE', #19883, #14402 ) ;
#16588 = ORIENTED_EDGE ( 'NONE', *, *, #17494, .F. ) ;
#16589 = ORIENTED_EDGE ( 'NONE', *, *, #20383, .T. ) ;
#16590 = CARTESIAN_POINT ( 'NONE',  ( 2.063750000000000195, 24.21318500000000284, 8.731249999999999289 ) ) ;
#16591 = CARTESIAN_POINT ( 'NONE',  ( 8.057976852920029742, 11.73130284909294119, 1.232157028814356403 ) ) ;
#16592 = CARTESIAN_POINT ( 'NONE',  ( 6.822572929214665294, 12.01675953414323139, 4.751156277397826422 ) ) ;
#16593 = VECTOR ( 'NONE', #4810, 1000.000000000000227 ) ;
#16594 = AXIS2_PLACEMENT_3D ( 'NONE', #17018, #101, #3326 ) ;
#16595 = CARTESIAN_POINT ( 'NONE',  ( 17.02725982432203367, -3.968114999999999615, -14.27444360421403857 ) ) ;
#16596 = CARTESIAN_POINT ( 'NONE',  ( 1.761257652907455062, 13.02131026627836086, 0.3965737215900302370 ) ) ;
#16597 = CARTESIAN_POINT ( 'NONE',  ( 0.1099108948849764067, 12.41872062087720607, 1.953321936160630434 ) ) ;
#16598 = ADVANCED_FACE ( 'NONE', ( #1776 ), #6645, .T. ) ;
#16599 = CARTESIAN_POINT ( 'NONE',  ( 39.62791084302666178, 34.52875999999999834, -24.65774797299118859 ) ) ;
#16600 = CIRCLE ( 'NONE', #17355, 1.984374999999998890 ) ;
#16601 = ORIENTED_EDGE ( 'NONE', *, *, #272, .F. ) ;
#16602 = CARTESIAN_POINT ( 'NONE',  ( -0.7122774860577034683, 19.84248487494580004, 3.546694122126617277 ) ) ;
#16603 = FACE_OUTER_BOUND ( 'NONE', #2327, .T. ) ;
#16604 = DIRECTION ( 'NONE',  ( -0.9685006480810791629, 0.000000000000000000, -0.2490110332224850231 ) ) ;
#16605 = CARTESIAN_POINT ( 'NONE',  ( 18.72668781722862263, -7.437140393198111710, -14.26808916428128349 ) ) ;
#16606 = CARTESIAN_POINT ( 'NONE',  ( -15.27766260488554195, -1.983739999999999393, -26.04727837583638461 ) ) ;
#16607 = ORIENTED_EDGE ( 'NONE', *, *, #15235, .F. ) ;
#16608 = CARTESIAN_POINT ( 'NONE',  ( 13.17436130925518967, 12.73805723869360129, 6.175612552832564717 ) ) ;
#16609 = CARTESIAN_POINT ( 'NONE',  ( 9.181556427945844590, 17.35025276895908064, -3.541092686917109766 ) ) ;
#16610 = ORIENTED_EDGE ( 'NONE', *, *, #13219, .T. ) ;
#16611 = TOROIDAL_SURFACE ( 'NONE', #3905, 3.174999999999999822, 0.5953125000000000222 ) ;
#16612 = CARTESIAN_POINT ( 'NONE',  ( 8.208960929233390047, 21.21049822788766193, 5.041055855688859388 ) ) ;
#16613 = CARTESIAN_POINT ( 'NONE',  ( 45.99559936598748777, 34.52875999999999834, 5.449572532947073000 ) ) ;
#16614 = CARTESIAN_POINT ( 'NONE',  ( 1.986054180200191643, 13.53163558985986192, 0.9852467751172055976 ) ) ;
#16615 = CYLINDRICAL_SURFACE ( 'NONE', #11666, 0.7950200000000010592 ) ;
#16616 = DIRECTION ( 'NONE',  ( 0.000000000000000000, -1.000000000000000000, 0.000000000000000000 ) ) ;
#16617 = EDGE_LOOP ( 'NONE', ( #3377, #13824, #15976, #3053 ) ) ;
#16618 = CARTESIAN_POINT ( 'NONE',  ( 9.415202144866304579, 11.84307591169006102, 5.174863401006513541 ) ) ;
#16619 = CIRCLE ( 'NONE', #3180, 0.7950200000000003930 ) ;
#16620 = CARTESIAN_POINT ( 'NONE',  ( 6.575770747954134521, 10.94213887786034078, 2.272703023869682148 ) ) ;
#16621 = CARTESIAN_POINT ( 'NONE',  ( 29.98909767165928386, 23.40768749999999798, -5.214162619065493054 ) ) ;
#16622 = EDGE_CURVE ( 'NONE', #13681, #21107, #6977, .T. ) ;
#16623 = DIRECTION ( 'NONE',  ( -0.7421532822901579785, 0.000000000000000000, 0.6702301885068628895 ) ) ;
#16624 = CARTESIAN_POINT ( 'NONE',  ( 6.694325579490929101, 11.08857721632392135, 2.712616371685049987 ) ) ;
#16625 = DIRECTION ( 'NONE',  ( -0.2868778675745010664, 0.000000000000000000, -0.9579671649362032637 ) ) ;
#16626 = FACE_OUTER_BOUND ( 'NONE', #11882, .T. ) ;
#16627 = DIRECTION ( 'NONE',  ( 0.000000000000000000, 1.000000000000000000, 0.000000000000000000 ) ) ;
#16628 = AXIS2_PLACEMENT_3D ( 'NONE', #6076, #12849, #19570 ) ;
#16629 = ORIENTED_EDGE ( 'NONE', *, *, #157, .F. ) ;
#16630 = CARTESIAN_POINT ( 'NONE',  ( 35.15748561355322011, 34.52875999999999834, 0.3244898641346534163 ) ) ;
#16631 = VECTOR ( 'NONE', #19419, 1000.000000000000114 ) ;
#16632 = CARTESIAN_POINT ( 'NONE',  ( 39.00487391863466513, 40.07742955315917044, -3.894748490060887747 ) ) ;
#16633 = FACE_OUTER_BOUND ( 'NONE', #11359, .T. ) ;
#16634 = CARTESIAN_POINT ( 'NONE',  ( 13.16830043700046460, 15.09637057925005799, 6.264522879333630279 ) ) ;
#16635 = DIRECTION ( 'NONE',  ( 0.000000000000000000, 1.000000000000000000, 0.000000000000000000 ) ) ;
#16636 = CARTESIAN_POINT ( 'NONE',  ( 20.35960306314353474, -3.328948665870211432, -15.28812545466150219 ) ) ;
#16637 = CARTESIAN_POINT ( 'NONE',  ( 34.72145145287101542, 34.52875999999999834, 0.5851394578805096947 ) ) ;
#16638 = ORIENTED_EDGE ( 'NONE', *, *, #21103, .T. ) ;
#16639 = FACE_OUTER_BOUND ( 'NONE', #5261, .T. ) ;
#16640 = EDGE_LOOP ( 'NONE', ( #5415, #12246 ) ) ;
#16641 = LINE ( 'NONE', #21614, #16056 ) ;
#16642 = VECTOR ( 'NONE', #14217, 1000.000000000000227 ) ;
#16643 = AXIS2_PLACEMENT_3D ( 'NONE', #15857, #12305, #12424 ) ;
#16644 = CARTESIAN_POINT ( 'NONE',  ( 21.56000048501562816, -3.394315525992640303, -15.42643609242808367 ) ) ;
#16645 = ORIENTED_EDGE ( 'NONE', *, *, #9399, .F. ) ;
#16646 = CARTESIAN_POINT ( 'NONE',  ( 5.594467393561600943, 13.98451010310800768, -0.8567667164377248401 ) ) ;
#16647 = VECTOR ( 'NONE', #2713, 1000.000000000000000 ) ;
#16648 = CARTESIAN_POINT ( 'NONE',  ( -4.157227781567939928, 22.62314500000000095, 0.1758860224507720060 ) ) ;
#16649 = CARTESIAN_POINT ( 'NONE',  ( 14.11562798333356916, 21.64660035503122160, 3.663432050408041096 ) ) ;
#16650 = EDGE_CURVE ( 'NONE', #16425, #1721, #18688, .T. ) ;
#16651 = AXIS2_PLACEMENT_3D ( 'NONE', #20656, #328, #12505 ) ;
#16652 = ADVANCED_FACE ( 'NONE', ( #4992, #20015 ), #125, .T. ) ;
#16653 = AXIS2_PLACEMENT_3D ( 'NONE', #16398, #12976, #7976 ) ;
#16654 = CARTESIAN_POINT ( 'NONE',  ( 18.39685687182289797, -6.445242814774206686, -15.58509951939779370 ) ) ;
#16655 = PRESENTATION_STYLE_ASSIGNMENT (( #9682 ) ) ;
#16656 = ORIENTED_EDGE ( 'NONE', *, *, #14300, .T. ) ;
#16657 = CARTESIAN_POINT ( 'NONE',  ( 8.659021043980340337, 20.69798781994444425, 0.5487958848404460577 ) ) ;
#16658 = CARTESIAN_POINT ( 'NONE',  ( 12.65941454051080406, 20.52367786489136137, 5.608094639784014568 ) ) ;
#16659 = CARTESIAN_POINT ( 'NONE',  ( 36.54633153140314761, -1.983739999999999393, -9.516661413425623550 ) ) ;
#16660 = ORIENTED_EDGE ( 'NONE', *, *, #19653, .T. ) ;
#16661 = ORIENTED_EDGE ( 'NONE', *, *, #11972, .T. ) ;
#16662 = AXIS2_PLACEMENT_3D ( 'NONE', #18249, #4775, #19788 ) ;
#16663 = DIRECTION ( 'NONE',  ( 0.000000000000000000, 1.000000000000000000, 0.000000000000000000 ) ) ;
#16665 = FACE_OUTER_BOUND ( 'NONE', #5585, .T. ) ;
#16664 = CARTESIAN_POINT ( 'NONE',  ( 5.535619616285561762, 15.64056738454816120, 8.892138302534441152 ) ) ;
#16666 = ORIENTED_EDGE ( 'NONE', *, *, #18950, .T. ) ;
#16667 = CARTESIAN_POINT ( 'NONE',  ( 7.125557253250215162, 19.02648549786798426, 7.691136940842363323 ) ) ;
#16668 = ORIENTED_EDGE ( 'NONE', *, *, #16898, .F. ) ;
#16669 = VECTOR ( 'NONE', #15827, 1000.000000000000000 ) ;
#16670 = ORIENTED_EDGE ( 'NONE', *, *, #9544, .F. ) ;
#16671 = VECTOR ( 'NONE', #15168, 1000.000000000000000 ) ;
#16672 = EDGE_CURVE ( 'NONE', #21532, #18768, #6876, .T. ) ;
#16673 = CARTESIAN_POINT ( 'NONE',  ( 0.1806150403938127091, 13.36329209284379793, 2.058942537303792619 ) ) ;
#16674 = CARTESIAN_POINT ( 'NONE',  ( 39.73003449695463019, 38.88803500000000213, -2.235125070556357674 ) ) ;
#16675 = ORIENTED_EDGE ( 'NONE', *, *, #5574, .F. ) ;
#16676 = VECTOR ( 'NONE', #12268, 1000.000000000000000 ) ;
#16677 = CARTESIAN_POINT ( 'NONE',  ( 11.40832977423153594, 17.71807980195418608, 7.511151340609421467 ) ) ;
#16678 = EDGE_CURVE ( 'NONE', #8026, #14393, #8636, .T. ) ;
#16679 = ADVANCED_FACE ( 'NONE', ( #3449 ), #3351, .F. ) ;
#16680 = DIRECTION ( 'NONE',  ( 0.000000000000000000, -1.000000000000000000, 0.000000000000000000 ) ) ;
#16681 = LINE ( 'NONE', #1522, #10389 ) ;
#16682 = DIRECTION ( 'NONE',  ( 0.000000000000000000, 1.000000000000000000, 0.000000000000000000 ) ) ;
#16683 = CARTESIAN_POINT ( 'NONE',  ( 2.295644084928958328, 19.71408608352444247, 0.5126537937488709895 ) ) ;
#16684 = AXIS2_PLACEMENT_3D ( 'NONE', #4195, #21318, #11260 ) ;
#16685 = CIRCLE ( 'NONE', #16704, 15.47812499999999680 ) ;
#16686 = EDGE_LOOP ( 'NONE', ( #628, #19441, #4368, #10026 ) ) ;
#16687 = DIRECTION ( 'NONE',  ( 0.000000000000000000, -1.000000000000000000, 0.000000000000000000 ) ) ;
#16688 = DIRECTION ( 'NONE',  ( -0.9685006480810792739, 0.000000000000000000, -0.2490110332224846346 ) ) ;
#16689 = DIRECTION ( 'NONE',  ( 0.000000000000000000, 0.000000000000000000, -1.000000000000000000 ) ) ;
#16690 = DIRECTION ( 'NONE',  ( 0.000000000000000000, 1.000000000000000000, 0.000000000000000000 ) ) ;
#16691 = ORIENTED_EDGE ( 'NONE', *, *, #1258, .F. ) ;
#16692 = ORIENTED_EDGE ( 'NONE', *, *, #2600, .T. ) ;
#16693 = CARTESIAN_POINT ( 'NONE',  ( 7.359377386964466083, 16.36402550683702373, -2.195284595531059590 ) ) ;
#16694 = DIRECTION ( 'NONE',  ( 0.000000000000000000, -1.000000000000000000, 0.000000000000000000 ) ) ;
#16695 = VERTEX_POINT ( 'NONE', #16927 ) ;
#16696 = AXIS2_PLACEMENT_3D ( 'NONE', #13213, #16737, #9853 ) ;
#16697 = ORIENTED_EDGE ( 'NONE', *, *, #20701, .F. ) ;
#16698 = LINE ( 'NONE', #14833, #20131 ) ;
#16699 = ORIENTED_EDGE ( 'NONE', *, *, #10606, .T. ) ;
#16700 = EDGE_CURVE ( 'NONE', #17229, #6182, #16731, .T. ) ;
#16701 = CARTESIAN_POINT ( 'NONE',  ( 8.734026292629820887, 11.84157558182232606, 4.211351354823381854 ) ) ;
#16702 = CARTESIAN_POINT ( 'NONE',  ( 6.671301235538900976, 11.80771363267201224, 4.070312667603704249 ) ) ;
#16703 = AXIS2_PLACEMENT_3D ( 'NONE', #16317, #7894, #18074 ) ;
#16704 = AXIS2_PLACEMENT_3D ( 'NONE', #12838, #13054, #21098 ) ;
#16705 = PLANE ( 'NONE',  #11298 ) ;
#16706 = AXIS2_PLACEMENT_3D ( 'NONE', #9184, #7753, #12417 ) ;
#16707 = CARTESIAN_POINT ( 'NONE',  ( -22.90596259062238005, -8.889364999999999739, -9.869321627248080375 ) ) ;
#16708 = DIRECTION ( 'NONE',  ( 0.000000000000000000, 1.000000000000000000, 0.000000000000000000 ) ) ;
#16709 = FACE_OUTER_BOUND ( 'NONE', #6264, .T. ) ;
#16710 = CARTESIAN_POINT ( 'NONE',  ( 0.2410472161520063328, 18.96554497951561302, 0.7464930760089547590 ) ) ;
#16711 = DIRECTION ( 'NONE',  ( 0.000000000000000000, -1.000000000000000000, 0.000000000000000000 ) ) ;
#16712 = ORIENTED_EDGE ( 'NONE', *, *, #1979, .F. ) ;
#16713 = CARTESIAN_POINT ( 'NONE',  ( 1.599345239557343090, 20.41800832758468331, 3.409096474281709810 ) ) ;
#16714 = CARTESIAN_POINT ( 'NONE',  ( 13.28822531734660828, 36.51313500000000545, -15.23578611614444078 ) ) ;
#16715 = CARTESIAN_POINT ( 'NONE',  ( -29.36874999999999858, 1.984375000000000000, -3.968750000000000000 ) ) ;
#16716 = DIRECTION ( 'NONE',  ( -0.7421532822901572013, 0.000000000000000000, 0.6702301885068637777 ) ) ;
#16717 = DIRECTION ( 'NONE',  ( 0.000000000000000000, -1.000000000000000000, -0.000000000000000000 ) ) ;
#16718 = ORIENTED_EDGE ( 'NONE', *, *, #13070, .T. ) ;
#16719 = CARTESIAN_POINT ( 'NONE',  ( 9.054956828960067483, 17.37326356681460382, -3.634900410956593664 ) ) ;
#16720 = AXIS2_PLACEMENT_3D ( 'NONE', #8092, #17956, #7886 ) ;
#16721 = CARTESIAN_POINT ( 'NONE',  ( 29.36874999999999858, 22.62187499999999929, 8.731249999999999289 ) ) ;
#16722 = CARTESIAN_POINT ( 'NONE',  ( 9.191111131702870196, 13.13842489233451616, -2.664320628172200944 ) ) ;
#16723 = CARTESIAN_POINT ( 'NONE',  ( 6.750174310882091078, 21.34127784185943000, 1.051171576271183072 ) ) ;
#16724 = CARTESIAN_POINT ( 'NONE',  ( 67.40134256979101224, 1.984375000000000000, -13.30734117861468135 ) ) ;
#16725 = LINE ( 'NONE', #18798, #9468 ) ;
#16726 = EDGE_CURVE ( 'NONE', #4424, #19957, #16729, .T. ) ;
#16727 = AXIS2_PLACEMENT_3D ( 'NONE', #17329, #8694, #15697 ) ;
#16728 = EDGE_CURVE ( 'NONE', #20833, #17882, #4794, .T. ) ;
#16729 = LINE ( 'NONE', #11631, #4010 ) ;
#16730 = VERTEX_POINT ( 'NONE', #18265 ) ;
#16731 = CIRCLE ( 'NONE', #6483, 3.970019999999997662 ) ;
#16732 = CARTESIAN_POINT ( 'NONE',  ( 9.682029097783299676, 17.29611120545237313, -3.402978531621489555 ) ) ;
#16733 = CARTESIAN_POINT ( 'NONE',  ( 5.277159435657938324, 13.56613987398194254, 7.097935826007862659 ) ) ;
#16734 = CARTESIAN_POINT ( 'NONE',  ( -15.41509608936259035, -4.609114529603660415, -10.31276839742836415 ) ) ;
#16735 = CARTESIAN_POINT ( 'NONE',  ( 0.9277850458616880847, 20.20533454244034033, 7.839724834913604390 ) ) ;
#16736 = CARTESIAN_POINT ( 'NONE',  ( 49.16323787629939801, 30.56064500000000095, -27.09503225884920141 ) ) ;
#16737 = DIRECTION ( 'NONE',  ( 0.2868778675745011220, 0.000000000000000000, 0.9579671649362034858 ) ) ;
#16738 = CARTESIAN_POINT ( 'NONE',  ( 29.19635173153840313, 30.56064500000000095, -6.218966092919240296 ) ) ;
#16739 = DIRECTION ( 'NONE',  ( 0.000000000000000000, 0.000000000000000000, 1.000000000000000000 ) ) ;
#16740 = CARTESIAN_POINT ( 'NONE',  ( 11.94887888776901441, -6.501231973260999553, -16.94794046497096573 ) ) ;
#16741 = CIRCLE ( 'NONE', #4734, 9.525000000000002132 ) ;
#16742 = DIRECTION ( 'NONE',  ( 0.2868778675745010664, 0.000000000000000000, 0.9579671649362032637 ) ) ;
#16743 = ORIENTED_EDGE ( 'NONE', *, *, #286, .T. ) ;
#16744 = CARTESIAN_POINT ( 'NONE',  ( 1.854799496439154316, 16.26393749999999727, 3.211081754263136911 ) ) ;
#16745 = DIRECTION ( 'NONE',  ( -0.000000000000000000, -1.000000000000000000, 0.000000000000000000 ) ) ;
#16746 = ORIENTED_EDGE ( 'NONE', *, *, #18458, .T. ) ;
#16747 = CARTESIAN_POINT ( 'NONE',  ( 13.16369351907254526, 14.77213119101223526, 6.175811950428527375 ) ) ;
#16748 = DIRECTION ( 'NONE',  ( 0.000000000000000000, 1.000000000000000000, 0.000000000000000000 ) ) ;
#16749 = CARTESIAN_POINT ( 'NONE',  ( 61.09555596642878328, -1.983739999999999837, -12.53419992421059348 ) ) ;
#16750 = CARTESIAN_POINT ( 'NONE',  ( 16.92054404696516912, 1.202889707813861619, -15.03119329449350339 ) ) ;
#16751 = FACE_OUTER_BOUND ( 'NONE', #7302, .T. ) ;
#16752 = AXIS2_PLACEMENT_3D ( 'NONE', #2424, #20763, #2084 ) ;
#16753 = ORIENTED_EDGE ( 'NONE', *, *, #1258, .T. ) ;
#16754 = CYLINDRICAL_SURFACE ( 'NONE', #17706, 19.05000000000000426 ) ;
#16755 = EDGE_CURVE ( 'NONE', #11247, #9392, #17429, .T. ) ;
#16756 = ORIENTED_EDGE ( 'NONE', *, *, #20360, .T. ) ;
#16757 = CARTESIAN_POINT ( 'NONE',  ( 6.008532079804368209, 11.28156496648768226, 2.932085512598874733 ) ) ;
#16758 = AXIS2_PLACEMENT_3D ( 'NONE', #383, #10336, #8668 ) ;
#16759 = ORIENTED_EDGE ( 'NONE', *, *, #1108, .T. ) ;
#16760 = CARTESIAN_POINT ( 'NONE',  ( 12.86918211560430514, 18.46417960692862437, 6.076019728440299694 ) ) ;
#16761 = CARTESIAN_POINT ( 'NONE',  ( 7.670774570915360968, 18.07295993736750361, -1.943745484816997937 ) ) ;
#16762 = CARTESIAN_POINT ( 'NONE',  ( 38.24361653725164700, 38.57685578888346356, -4.842928593324986153 ) ) ;
#16763 = CARTESIAN_POINT ( 'NONE',  ( 5.633227044593422939, 12.08264022589296260, -0.3004653588455272750 ) ) ;
#16764 = AXIS2_PLACEMENT_3D ( 'NONE', #7771, #18170, #6321 ) ;
#16765 = CARTESIAN_POINT ( 'NONE',  ( 15.16174527195880017, -7.152427045711343467, -16.25377686098167374 ) ) ;
#16766 = PLANE ( 'NONE',  #8721 ) ;
#16767 = VERTEX_POINT ( 'NONE', #11749 ) ;
#16768 = CARTESIAN_POINT ( 'NONE',  ( 8.501344007088352583, 20.47739890484253067, 0.1352862916589856745 ) ) ;
#16769 = CARTESIAN_POINT ( 'NONE',  ( 8.817286373918717501, 20.20007397076694033, 6.586875430813535992 ) ) ;
#16770 = CARTESIAN_POINT ( 'NONE',  ( 38.96848998618624904, -5.166360000000000063, -3.934807454472129429 ) ) ;
#16771 = ORIENTED_EDGE ( 'NONE', *, *, #9625, .T. ) ;
#16772 = ORIENTED_EDGE ( 'NONE', *, *, #3867, .T. ) ;
#16773 = DIRECTION ( 'NONE',  ( 1.000000000000000000, 0.000000000000000000, 0.000000000000000000 ) ) ;
#16775 = CARTESIAN_POINT ( 'NONE',  ( 67.40134256979101224, 1.984375000000000000, -13.30734117861468135 ) ) ;
#16774 = CARTESIAN_POINT ( 'NONE',  ( 5.063315581345954719, 19.21739139815786146, 8.104051299585993462 ) ) ;
#16776 = VERTEX_POINT ( 'NONE', #13634 ) ;
#16777 = CARTESIAN_POINT ( 'NONE',  ( 7.017698028421007095, 19.43385999692815602, 7.433407674448314850 ) ) ;
#16778 = ORIENTED_EDGE ( 'NONE', *, *, #18379, .F. ) ;
#16779 = ADVANCED_FACE ( 'NONE', ( #17043 ), #3123, .F. ) ;
#16780 = VERTEX_POINT ( 'NONE', #8311 ) ;
#16781 = DIRECTION ( 'NONE',  ( -0.000000000000000000, -1.000000000000000000, 0.000000000000000000 ) ) ;
#16782 = ORIENTED_EDGE ( 'NONE', *, *, #339, .T. ) ;
#16783 = CIRCLE ( 'NONE', #12192, 0.5079999999999984528 ) ;
#16784 = CARTESIAN_POINT ( 'NONE',  ( 11.23451117572187918, 16.27132894921272310, -4.476865026338582076 ) ) ;
#16785 = FACE_OUTER_BOUND ( 'NONE', #6283, .T. ) ;
#16786 = DIRECTION ( 'NONE',  ( 0.4080888115384288528, 0.000000000000000000, 0.9129422336036122632 ) ) ;
#16787 = CARTESIAN_POINT ( 'NONE',  ( 1.659792374793198411, 15.50571454768893709, -0.6235934458232202937 ) ) ;
#16788 = ORIENTED_EDGE ( 'NONE', *, *, #13005, .F. ) ;
#16789 = CARTESIAN_POINT ( 'NONE',  ( -17.46249999999999858, 0.000000000000000000, 0.000000000000000000 ) ) ;
#16790 = FACE_OUTER_BOUND ( 'NONE', #11361, .T. ) ;
#16791 = FACE_BOUND ( 'NONE', #8959, .T. ) ;
#16792 = EDGE_CURVE ( 'NONE', #2731, #6613, #2957, .T. ) ;
#16793 = LINE ( 'NONE', #13376, #19719 ) ;
#16794 = VERTEX_POINT ( 'NONE', #9970 ) ;
#16795 = ORIENTED_EDGE ( 'NONE', *, *, #20748, .F. ) ;
#16796 = CARTESIAN_POINT ( 'NONE',  ( 5.473594542650097594, 15.56639808041640372, -1.390812284269987265 ) ) ;
#16797 = DIRECTION ( 'NONE',  ( 0.000000000000000000, 1.000000000000000000, 0.000000000000000000 ) ) ;
#16798 = ORIENTED_EDGE ( 'NONE', *, *, #7660, .T. ) ;
#16799 = VERTEX_POINT ( 'NONE', #19140 ) ;
#16800 = CARTESIAN_POINT ( 'NONE',  ( 18.65312499999999929, 32.54502000000000095, 5.159374999999999822 ) ) ;
#16801 = ADVANCED_FACE ( 'NONE', ( #10634 ), #8965, .T. ) ;
#16802 = ORIENTED_EDGE ( 'NONE', *, *, #14515, .T. ) ;
#16803 = EDGE_CURVE ( 'NONE', #7335, #15942, #15616, .T. ) ;
#16804 = ADVANCED_FACE ( 'NONE', ( #10415 ), #572, .F. ) ;
#16805 = CARTESIAN_POINT ( 'NONE',  ( 8.566873072168270653, 11.62770347711273011, 3.469410504889820501 ) ) ;
#16806 = DIRECTION ( 'NONE',  ( -0.000000000000000000, -1.000000000000000000, 0.000000000000000000 ) ) ;
#16807 = LINE ( 'NONE', #8718, #7243 ) ;
#16808 = CARTESIAN_POINT ( 'NONE',  ( 0.06308363157408580779, 12.60631702034428692, 1.730364172241236620 ) ) ;
#16809 = PLANE ( 'NONE',  #15824 ) ;
#16810 = VERTEX_POINT ( 'NONE', #12411 ) ;
#16811 = CARTESIAN_POINT ( 'NONE',  ( 1.820434556146364402, 15.68905071955487962, 8.881803553093584824 ) ) ;
#16812 = CARTESIAN_POINT ( 'NONE',  ( 67.79270099634359781, 32.54502000000000095, -13.76558698117381851 ) ) ;
#16813 = DIRECTION ( 'NONE',  ( 0.000000000000000000, -1.000000000000000000, -0.000000000000000000 ) ) ;
#16814 = CARTESIAN_POINT ( 'NONE',  ( 29.15193331460030279, -6.752907499999998286, -13.61707959051006966 ) ) ;
#16815 = ADVANCED_FACE ( 'NONE', ( #17596 ), #7419, .T. ) ;
#16816 = DIRECTION ( 'NONE',  ( 0.000000000000000000, 1.000000000000000000, 0.000000000000000000 ) ) ;
#16817 = ORIENTED_EDGE ( 'NONE', *, *, #14799, .T. ) ;
#16818 = CARTESIAN_POINT ( 'NONE',  ( 9.198936130449542503, 14.67110634242510159, 7.858938460866098374 ) ) ;
#16819 = CARTESIAN_POINT ( 'NONE',  ( 13.31981936710468339, 16.89510937500811849, 7.147718160282645172 ) ) ;
#16820 = ORIENTED_EDGE ( 'NONE', *, *, #2466, .T. ) ;
#16821 = CARTESIAN_POINT ( 'NONE',  ( 8.669746721805902112, 10.90552857616499161, 3.865604682332115516 ) ) ;
#16822 = LINE ( 'NONE', #1342, #7746 ) ;
#16823 = DIRECTION ( 'NONE',  ( 0.3697464814795228816, -0.9291326812858931028, 0.000000000000000000 ) ) ;
#16824 = ADVANCED_FACE ( 'NONE', ( #1997 ), #12524, .T. ) ;
#16825 = LINE ( 'NONE', #8087, #5287 ) ;
#16826 = CARTESIAN_POINT ( 'NONE',  ( 26.59062499999999929, 30.56064500000000095, 8.731249999999999289 ) ) ;
#16827 = AXIS2_PLACEMENT_3D ( 'NONE', #6126, #17861, #19824 ) ;
#16828 = CARTESIAN_POINT ( 'NONE',  ( 5.869188306888136530, 15.50533030672313828, -1.931863268461263106 ) ) ;
#16829 = CARTESIAN_POINT ( 'NONE',  ( 5.194454836083180815, 13.07028570565210224, 6.652979041940234595 ) ) ;
#16830 = CARTESIAN_POINT ( 'NONE',  ( 5.573107417874706648, 17.51139020089073028, 8.753967866118298247 ) ) ;
#16831 = LINE ( 'NONE', #21701, #19168 ) ;
#16832 = CARTESIAN_POINT ( 'NONE',  ( 20.24085330020690066, -1.338735640124543602, -14.75261804466661353 ) ) ;
#16833 = CARTESIAN_POINT ( 'NONE',  ( 0.4276177683824305409, 12.38241104890028232, 3.439344687585752514 ) ) ;
#16834 = LINE ( 'NONE', #18375, #11857 ) ;
#16835 = CARTESIAN_POINT ( 'NONE',  ( 18.11329111247768253, -7.967937188882820543, -15.61660755156637315 ) ) ;
#16836 = EDGE_CURVE ( 'NONE', #2732, #8399, #6113, .T. ) ;
#16837 = EDGE_CURVE ( 'NONE', #9905, #3908, #11425, .T. ) ;
#16838 = EDGE_CURVE ( 'NONE', #5344, #20691, #3893, .T. ) ;
#16839 = ORIENTED_EDGE ( 'NONE', *, *, #15086, .F. ) ;
#16840 = LINE ( 'NONE', #11764, #6082 ) ;
#16841 = CARTESIAN_POINT ( 'NONE',  ( 8.692131961109870630, 21.56859194724540174, 0.5848482333739358774 ) ) ;
#16842 = DIRECTION ( 'NONE',  ( 0.2490110332224857170, 0.000000000000000000, -0.9685006480810790519 ) ) ;
#16843 = ORIENTED_EDGE ( 'NONE', *, *, #7074, .F. ) ;
#16844 = CARTESIAN_POINT ( 'NONE',  ( 13.06483546133407891, 17.09753932500757756, 6.359823774401709429 ) ) ;
#16845 = VECTOR ( 'NONE', #13172, 1000.000000000000114 ) ;
#16846 = DIRECTION ( 'NONE',  ( 1.000000000000000000, 0.000000000000000000, 0.000000000000000000 ) ) ;
#16847 = CARTESIAN_POINT ( 'NONE',  ( 14.79613284372093318, -7.415112926742073896, -14.97538028618549610 ) ) ;
#16849 = FACE_OUTER_BOUND ( 'NONE', #17840, .T. ) ;
#16848 = CARTESIAN_POINT ( 'NONE',  ( 4.747186406083175214, 20.72645064840772022, 2.280034233475693117 ) ) ;
#16850 = VERTEX_POINT ( 'NONE', #13977 ) ;
#16851 = DIRECTION ( 'NONE',  ( 1.000000000000000000, 0.000000000000000000, 0.000000000000000000 ) ) ;
#16852 = DIRECTION ( 'NONE',  ( 0.000000000000000000, 1.000000000000000000, 0.000000000000000000 ) ) ;
#16853 = CARTESIAN_POINT ( 'NONE',  ( 42.79471501377724252, 34.52875999999999834, 5.049205022181460834 ) ) ;
#16854 = CARTESIAN_POINT ( 'NONE',  ( 6.015389740508374494, 11.22565445350847213, 2.925956496411346475 ) ) ;
#16855 = ORIENTED_EDGE ( 'NONE', *, *, #17014, .F. ) ;
#16856 = CARTESIAN_POINT ( 'NONE',  ( 10.66741777435992233, 21.11777521280046344, 0.3018417449422642895 ) ) ;
#16857 = CARTESIAN_POINT ( 'NONE',  ( 9.031267397129903785, 18.23281813489354164, 6.939219899636122513 ) ) ;
#16858 = CARTESIAN_POINT ( 'NONE',  ( 1.567589786362412196, 18.89460405061472414, 8.826553739152313227 ) ) ;
#16859 = CARTESIAN_POINT ( 'NONE',  ( 6.238925459287739450, 20.69394519596638204, -0.2505430798033594364 ) ) ;
#16860 = CIRCLE ( 'NONE', #2751, 0.7950199999999986167 ) ;
#16861 = CARTESIAN_POINT ( 'NONE',  ( 11.94302826524597805, -3.805938227851652478, -16.84833834122463614 ) ) ;
#16862 = EDGE_CURVE ( 'NONE', #16009, #12286, #18446, .T. ) ;
#16863 = CARTESIAN_POINT ( 'NONE',  ( 31.06384331886062711, -5.959792500000001603, 1.146004012482531476 ) ) ;
#16864 = ORIENTED_EDGE ( 'NONE', *, *, #19455, .T. ) ;
#16865 = CARTESIAN_POINT ( 'NONE',  ( 9.417227436378860617, 21.07740322983227443, 2.575106661504599881 ) ) ;
#16866 = CARTESIAN_POINT ( 'NONE',  ( 5.436098872970559270, 13.59057812530450171, -1.547591233524117982 ) ) ;
#16867 = CARTESIAN_POINT ( 'NONE',  ( 1.854799496439154316, 13.08893749999999834, 3.211081754263136911 ) ) ;
#16868 = ORIENTED_EDGE ( 'NONE', *, *, #14301, .F. ) ;
#16869 = VERTEX_POINT ( 'NONE', #20675 ) ;
#16870 = DIRECTION ( 'NONE',  ( 0.7334850928793775759, 0.6768732144311021548, -0.06198604769976992501 ) ) ;
#16871 = CARTESIAN_POINT ( 'NONE',  ( 10.92301329967130030, 14.92480105555379488, -4.179632980644835349 ) ) ;
#16873 = DIRECTION ( 'NONE',  ( 0.000000000000000000, -1.000000000000000000, -0.000000000000000000 ) ) ;
#16872 = CARTESIAN_POINT ( 'NONE',  ( 4.834045568277948846, 19.16583807351516100, 8.093579589020821530 ) ) ;
#16874 = ORIENTED_EDGE ( 'NONE', *, *, #12768, .F. ) ;
#16875 = CARTESIAN_POINT ( 'NONE',  ( 5.015481723962230021, 21.32780660904764858, 2.079200966080708479 ) ) ;
#16876 = DIRECTION ( 'NONE',  ( -0.2490110332224850509, 0.000000000000000000, 0.9685006480810792739 ) ) ;
#16877 = ORIENTED_EDGE ( 'NONE', *, *, #7880, .T. ) ;
#16878 = CARTESIAN_POINT ( 'NONE',  ( -22.75431282566211522, 40.79338547039380103, -25.41543459098148716 ) ) ;
#16879 = ORIENTED_EDGE ( 'NONE', *, *, #13318, .T. ) ;
#16880 = DIRECTION ( 'NONE',  ( 0.000000000000000000, 1.000000000000000000, 0.000000000000000000 ) ) ;
#16881 = CARTESIAN_POINT ( 'NONE',  ( 37.13209340688868565, -6.356984999999999886, -3.529402718062123689 ) ) ;
#16882 = DIRECTION ( 'NONE',  ( -0.000000000000000000, -1.000000000000000000, 0.000000000000000000 ) ) ;
#16883 = CARTESIAN_POINT ( 'NONE',  ( 2.775292155461787758, 20.75260234445946850, 1.748868790410040619 ) ) ;
#16884 = EDGE_CURVE ( 'NONE', #7791, #14366, #16379, .T. ) ;
#16885 = ORIENTED_EDGE ( 'NONE', *, *, #9837, .T. ) ;
#16886 = CARTESIAN_POINT ( 'NONE',  ( 56.91751438644678984, 34.52875999999999834, -20.96198986413465448 ) ) ;
#16887 = LINE ( 'NONE', #20850, #12091 ) ;
#16888 = CARTESIAN_POINT ( 'NONE',  ( 11.24737647850577993, 13.08957250000000094, -3.746985211334052046 ) ) ;
#16889 = DIRECTION ( 'NONE',  ( -0.6702301885068630005, 0.000000000000000000, -0.7421532822901580895 ) ) ;
#16891 = CARTESIAN_POINT ( 'NONE',  ( 18.89948197725901124, -5.655894340861864933, -14.27920814860754817 ) ) ;
#16890 = CARTESIAN_POINT ( 'NONE',  ( -20.63749999999999929, 16.27314499999999953, 10.71562499999999929 ) ) ;
#16892 = ORIENTED_EDGE ( 'NONE', *, *, #15235, .T. ) ;
#16893 = VERTEX_POINT ( 'NONE', #12293 ) ;
#16894 = CARTESIAN_POINT ( 'NONE',  ( 12.13375240738266214, 11.13394627749852361, 2.666777367712576119 ) ) ;
#16895 =( GEOMETRIC_REPRESENTATION_CONTEXT ( 3 ) GLOBAL_UNCERTAINTY_ASSIGNED_CONTEXT ( ( #17631 ) ) GLOBAL_UNIT_ASSIGNED_CONTEXT ( ( #6573, #18193, #21607 ) ) REPRESENTATION_CONTEXT ( 'NONE', 'WORKASPACE' ) );
#16896 = CARTESIAN_POINT ( 'NONE',  ( 3.568489545713221300, 13.11399658182230077, 8.209792117522704658 ) ) ;
#16897 = EDGE_LOOP ( 'NONE', ( #963, #4739, #13262, #18359, #7896 ) ) ;
#16898 = EDGE_CURVE ( 'NONE', #14819, #17008, #21291, .T. ) ;
#16899 = ORIENTED_EDGE ( 'NONE', *, *, #5242, .F. ) ;
#16900 = CARTESIAN_POINT ( 'NONE',  ( 49.16323787629939801, 0.000000000000000000, -27.09503225884920141 ) ) ;
#16901 = ORIENTED_EDGE ( 'NONE', *, *, #5817, .T. ) ;
#16902 = CARTESIAN_POINT ( 'NONE',  ( 9.249936709118586009, 16.07436072946943284, 7.222823812574241664 ) ) ;
#16903 = DIRECTION ( 'NONE',  ( 0.000000000000000000, 1.000000000000000000, 0.000000000000000000 ) ) ;
#16904 = DIRECTION ( 'NONE',  ( 0.2490110332224850509, 0.000000000000000000, -0.9685006480810792739 ) ) ;
#16905 = CARTESIAN_POINT ( 'NONE',  ( 60.38511073144201191, 32.54502000000000095, -22.26373525985038526 ) ) ;
#16906 = CARTESIAN_POINT ( 'NONE',  ( 0.2530718558280443675, 19.01130769708743173, 0.7743534949120846056 ) ) ;
#16907 = EDGE_CURVE ( 'NONE', #7705, #17225, #21019, .T. ) ;
#16908 = EDGE_CURVE ( 'NONE', #6167, #2495, #5650, .T. ) ;
#16909 = B_SPLINE_CURVE_WITH_KNOTS ( 'NONE', 3,
 ( #19082, #4253, #930, #21475, #6452, #3246, #3362, #1254, #18180, #10090 ),
 .UNSPECIFIED., .F., .F.,
 ( 4, 2, 2, 2, 4 ),
 ( 0.003573252179933841116, 0.004059386830566638800, 0.004545521481199436484, 0.005031656131832235035, 0.005517790782465032719 ),
 .UNSPECIFIED. ) ;
#16910 = ORIENTED_EDGE ( 'NONE', *, *, #21709, .F. ) ;
#16911 = CARTESIAN_POINT ( 'NONE',  ( 6.399950078107855767, 11.66082179432958377, 2.440713941562763445 ) ) ;
#16912 = LINE ( 'NONE', #20104, #20876 ) ;
#16913 = CARTESIAN_POINT ( 'NONE',  ( 52.25311689352595579, -6.512906051756550241, -17.53621019291011152 ) ) ;
#16914 = CARTESIAN_POINT ( 'NONE',  ( 32.42378190387104553, 0.000000000000000000, -18.15178106273469183 ) ) ;
#16915 = ORIENTED_EDGE ( 'NONE', *, *, #1924, .T. ) ;
#16916 = CARTESIAN_POINT ( 'NONE',  ( 10.11714758980606099, 20.94030016091612367, 5.401611073718733280 ) ) ;
#16917 = CIRCLE ( 'NONE', #16156, 9.525000000000000355 ) ;
#16918 = CARTESIAN_POINT ( 'NONE',  ( 52.44708915697334106, 34.52875999999999834, 4.020247972991190188 ) ) ;
#16919 = CARTESIAN_POINT ( 'NONE',  ( 12.71023870408584777, 20.14709925075540653, 5.798634777724255507 ) ) ;
#16920 = ORIENTED_EDGE ( 'NONE', *, *, #7913, .F. ) ;
#16921 = AXIS2_PLACEMENT_3D ( 'NONE', #8676, #10456, #10560 ) ;
#16922 = CARTESIAN_POINT ( 'NONE',  ( 9.426324800990981245, 13.63054490249874995, 7.306473834158507152 ) ) ;
#16923 = CARTESIAN_POINT ( 'NONE',  ( 6.097718537102145397, 12.01182390341870310, 1.432571743024261490 ) ) ;
#16924 = AXIS2_PLACEMENT_3D ( 'NONE', #15184, #2452, #19249 ) ;
#16925 = FACE_OUTER_BOUND ( 'NONE', #14060, .T. ) ;
#16926 = CARTESIAN_POINT ( 'NONE',  ( 1.092213287054645487, 20.02445172838347887, 2.973282941953453218 ) ) ;
#16927 = CARTESIAN_POINT ( 'NONE',  ( 17.87574706213523612, 36.51313500000000545, -11.18912023382283571 ) ) ;
#16928 = ADVANCED_FACE ( 'NONE', ( #12075 ), #2335, .T. ) ;
#16929 = CARTESIAN_POINT ( 'NONE',  ( 13.82166201609697609, 21.49735766717988383, 2.189693031311231053 ) ) ;
#16930 = CARTESIAN_POINT ( 'NONE',  ( 6.082277496570703157, 11.26983891803934235, 1.116890723640061145 ) ) ;
#16931 = CARTESIAN_POINT ( 'NONE',  ( 12.02474915109715603, 36.51313500000000545, -13.51434638588835391 ) ) ;
#16932 = ADVANCED_FACE ( 'NONE', ( #19247 ), #10847, .T. ) ;
#16933 = CARTESIAN_POINT ( 'NONE',  ( 19.74554184638576260, 0.02755205230605372105, -14.88057453995056889 ) ) ;
#16934 = VECTOR ( 'NONE', #4901, 1000.000000000000227 ) ;
#16935 = CARTESIAN_POINT ( 'NONE',  ( 2.171297880429710059, 12.53189561649392125, 2.160350752502488536 ) ) ;
#16936 = DIRECTION ( 'NONE',  ( 0.000000000000000000, 1.000000000000000000, 0.000000000000000000 ) ) ;
#16937 = CARTESIAN_POINT ( 'NONE',  ( 11.77229620076644956, -6.258712276749109016, -16.98231560743968416 ) ) ;
#16938 = AXIS2_PLACEMENT_3D ( 'NONE', #19018, #9293, #9179 ) ;
#16939 = PRESENTATION_STYLE_ASSIGNMENT (( #5006 ) ) ;
#16940 = EDGE_LOOP ( 'NONE', ( #7625, #18525, #11348, #7911 ) ) ;
#16941 = CARTESIAN_POINT ( 'NONE',  ( 10.99397269632869012, 12.69350398869253205, 5.272832363251270138 ) ) ;
#16942 = CARTESIAN_POINT ( 'NONE',  ( 10.77664050532247941, 20.02775797062505703, 6.254703954331844784 ) ) ;
#16943 = LINE ( 'NONE', #13759, #21767 ) ;
#16944 = FACE_BOUND ( 'NONE', #10401, .T. ) ;
#16945 = CARTESIAN_POINT ( 'NONE',  ( 12.88838202479853834, 18.27243614694899776, 6.040255587177526309 ) ) ;
#16946 = VECTOR ( 'NONE', #7877, 1000.000000000000000 ) ;
#16947 = CARTESIAN_POINT ( 'NONE',  ( 28.56548256563643662, -1.983739999999999393, -12.12873025803960658 ) ) ;
#16949 = CARTESIAN_POINT ( 'NONE',  ( 31.75000000000000000, 30.56064500000000095, -4.317999999999999616 ) ) ;
#16948 = CARTESIAN_POINT ( 'NONE',  ( -0.8930781184004659146, 19.84248487494580004, 3.600837626999320751 ) ) ;
#16950 = ORIENTED_EDGE ( 'NONE', *, *, #21445, .T. ) ;
#16951 = CARTESIAN_POINT ( 'NONE',  ( 49.13030338002142372, 109.3223030719999969, -2.154981381712871791 ) ) ;
#16952 = CARTESIAN_POINT ( 'NONE',  ( 4.138389979685599407, 18.66904148099360583, -0.05536455928733001464 ) ) ;
#16953 = LINE ( 'NONE', #16853, #2421 ) ;
#16954 = CIRCLE ( 'NONE', #19427, 0.5080000000000005622 ) ;
#16955 = CARTESIAN_POINT ( 'NONE',  ( 6.061592232884255083, 11.51780679014957087, 2.933444363316426440 ) ) ;
#16956 = EDGE_CURVE ( 'NONE', #374, #8103, #8361, .T. ) ;
#16957 = VECTOR ( 'NONE', #7782, 1000.000000000000114 ) ;
#16958 = EDGE_CURVE ( 'NONE', #5690, #11670, #18472, .T. ) ;
#16959 = EDGE_CURVE ( 'NONE', #1266, #11872, #4331, .T. ) ;
#16960 = ORIENTED_EDGE ( 'NONE', *, *, #20410, .F. ) ;
#16961 = CARTESIAN_POINT ( 'NONE',  ( 8.995636894096717739, 18.23281813489354164, 6.949889996801141834 ) ) ;
#16962 = CARTESIAN_POINT ( 'NONE',  ( 3.394140864483894848, 20.53104011336272094, 3.431716963511205254 ) ) ;
#16963 = CARTESIAN_POINT ( 'NONE',  ( 11.36309470493123897, 18.10709300986449222, -3.422778098908139555 ) ) ;
#16964 = CARTESIAN_POINT ( 'NONE',  ( 2.171104116788205030, 14.75527451915623267, -0.2596362615752321190 ) ) ;
#16965 = CARTESIAN_POINT ( 'NONE',  ( 10.93146967960046823, 19.57756785145604184, 6.739420547765535119 ) ) ;
#16966 = CIRCLE ( 'NONE', #7437, 0.7950200000000007261 ) ;
#16967 = VECTOR ( 'NONE', #16873, 1000.000000000000000 ) ;
#16968 = LINE ( 'NONE', #8890, #3183 ) ;
#16969 = ORIENTED_EDGE ( 'NONE', *, *, #12926, .T. ) ;
#16970 = CARTESIAN_POINT ( 'NONE',  ( 10.99993813090866723, 17.89902992434649676, 6.574171548972360668 ) ) ;
#16971 = CARTESIAN_POINT ( 'NONE',  ( 8.656775701180432492, 10.74414689430484238, 3.683671093170405086 ) ) ;
#16972 = VERTEX_POINT ( 'NONE', #13152 ) ;
#16973 = ORIENTED_EDGE ( 'NONE', *, *, #15492, .T. ) ;
#16974 = CARTESIAN_POINT ( 'NONE',  ( 47.80475250345343596, -5.166360000000002728, -11.91473563638196786 ) ) ;
#16976 = CARTESIAN_POINT ( 'NONE',  ( 17.22522857595987844, 36.51313500000000545, -15.04442098945225403 ) ) ;
#16975 = CARTESIAN_POINT ( 'NONE',  ( 2.687727953910716838, 19.71984925633132235, 8.028051864564421436 ) ) ;
#16977 = VERTEX_POINT ( 'NONE', #19970 ) ;
#16978 = CARTESIAN_POINT ( 'NONE',  ( 7.314098963983371782, 18.09774034698478218, 8.106240407049199348 ) ) ;
#16979 = VECTOR ( 'NONE', #369, 1000.000000000000000 ) ;
#16980 = CARTESIAN_POINT ( 'NONE',  ( 71.03305177384599745, 0.000000000000000000, -10.93409647675949969 ) ) ;
#16981 = AXIS2_PLACEMENT_3D ( 'NONE', #17764, #9342, #18195 ) ;
#16982 = ORIENTED_EDGE ( 'NONE', *, *, #4647, .T. ) ;
#16983 = AXIS2_PLACEMENT_3D ( 'NONE', #15026, #11358, #20062 ) ;
#16984 = EDGE_CURVE ( 'NONE', #1768, #10491, #8583, .T. ) ;
#16985 = EDGE_CURVE ( 'NONE', #12465, #2216, #17070, .T. ) ;
#16986 = CARTESIAN_POINT ( 'NONE',  ( 21.03437500000000071, 0.000000000000000000, 5.159374999999999822 ) ) ;
#16987 = ORIENTED_EDGE ( 'NONE', *, *, #20989, .F. ) ;
#16988 = CARTESIAN_POINT ( 'NONE',  ( 39.16413618835606769, 2.586003464000000029, -24.45043885672975392 ) ) ;
#16989 = PLANE ( 'NONE',  #15913 ) ;
#16990 = DIRECTION ( 'NONE',  ( 0.000000000000000000, -1.000000000000000000, 0.000000000000000000 ) ) ;
#16991 = CARTESIAN_POINT ( 'NONE',  ( 1.872722183360863157, 17.96163139729105396, -0.4538458379064382875 ) ) ;
#16992 = DIRECTION ( 'NONE',  ( -0.000000000000000000, -1.000000000000000000, 0.000000000000000000 ) ) ;
#16993 = VECTOR ( 'NONE', #7429, 999.9999999999998863 ) ;
#16994 = AXIS2_PLACEMENT_3D ( 'NONE', #10838, #17915, #17814 ) ;
#16995 = ORIENTED_EDGE ( 'NONE', *, *, #2974, .T. ) ;
#16996 = CARTESIAN_POINT ( 'NONE',  ( 48.78323016782857735, 32.54502000000000095, -25.79158832643865651 ) ) ;
#16997 = DIRECTION ( 'NONE',  ( 0.000000000000000000, 1.000000000000000000, 0.000000000000000000 ) ) ;
#16998 = CARTESIAN_POINT ( 'NONE',  ( -3.845402119898529758, 2.373947500000000765, -31.39393985263922460 ) ) ;
#17000 = CARTESIAN_POINT ( 'NONE',  ( 12.65199039493287358, -5.861692353372749409, -15.54496691525876528 ) ) ;
#16999 = DIRECTION ( 'NONE',  ( 0.000000000000000000, 1.000000000000000000, 0.000000000000000000 ) ) ;
#17001 = ORIENTED_EDGE ( 'NONE', *, *, #8176, .T. ) ;
#17002 = ORIENTED_EDGE ( 'NONE', *, *, #5327, .F. ) ;
#17003 = CIRCLE ( 'NONE', #4991, 0.5079999999999996740 ) ;
#17004 = CARTESIAN_POINT ( 'NONE',  ( 9.151378930904229492, 16.57955862325433571, 7.339540571888535148 ) ) ;
#17006 = DIRECTION ( 'NONE',  ( -0.9943660382494290406, 0.000000000000000000, 0.1060008583745199739 ) ) ;
#17005 = CARTESIAN_POINT ( 'NONE',  ( 6.751629654752353105, 10.91861244885538085, 4.241390806295360250 ) ) ;
#17007 = VERTEX_POINT ( 'NONE', #19348 ) ;
#17008 = VERTEX_POINT ( 'NONE', #17709 ) ;
#17009 = FACE_OUTER_BOUND ( 'NONE', #18831, .T. ) ;
#17010 = ORIENTED_EDGE ( 'NONE', *, *, #20701, .T. ) ;
#17011 = CARTESIAN_POINT ( 'NONE',  ( 7.478304415730235633, 16.36322443626852419, -2.127097502218570746 ) ) ;
#17012 = CARTESIAN_POINT ( 'NONE',  ( 6.396056618077795797, 11.71523274630726164, 2.847703469759983008 ) ) ;
#17013 = CIRCLE ( 'NONE', #5717, 9.524999999999996803 ) ;
#17014 = EDGE_CURVE ( 'NONE', #6031, #17792, #7544, .T. ) ;
#17015 = VECTOR ( 'NONE', #16689, 1000.000000000000000 ) ;
#17016 = CIRCLE ( 'NONE', #13155, 0.7950200000000005041 ) ;
#17017 = AXIS2_PLACEMENT_3D ( 'NONE', #11380, #5846, #12604 ) ;
#17018 = CARTESIAN_POINT ( 'NONE',  ( 34.84490081146155660, 0.000000000000000000, -0.2108409695808725060 ) ) ;
#17019 = ADVANCED_FACE ( 'NONE', ( #18318, #21747 ), #9908, .T. ) ;
#17020 = CARTESIAN_POINT ( 'NONE',  ( 13.28822531734660828, 36.51313500000000545, -15.23578611614444078 ) ) ;
#17021 = CARTESIAN_POINT ( 'NONE',  ( -0.1736154422522359353, 14.44032826713222128, 0.4251795190948972070 ) ) ;
#17022 = CARTESIAN_POINT ( 'NONE',  ( 1.268730000000000135, 9.129395000000000593, 10.65596716962832069 ) ) ;
#17023 = ORIENTED_EDGE ( 'NONE', *, *, #2288, .F. ) ;
#17024 = CARTESIAN_POINT ( 'NONE',  ( 3.802763359353439121, 15.57349433917940651, -0.7085367696333115806 ) ) ;
#17025 = DIRECTION ( 'NONE',  ( 0.000000000000000000, 1.000000000000000000, 0.000000000000000000 ) ) ;
#17026 = CARTESIAN_POINT ( 'NONE',  ( 55.56250000000000000, 0.000000000000000000, -10.31874999999999964 ) ) ;
#17027 = DIRECTION ( 'NONE',  ( 0.000000000000000000, 1.000000000000000000, 0.000000000000000000 ) ) ;
#17028 = DIRECTION ( 'NONE',  ( 0.000000000000000000, 1.000000000000000000, 0.000000000000000000 ) ) ;
#17029 = AXIS2_PLACEMENT_3D ( 'NONE', #15798, #8913, #3951 ) ;
#17030 = VERTEX_POINT ( 'NONE', #2560 ) ;
#17031 = CARTESIAN_POINT ( 'NONE',  ( 6.588601868897780989, 21.50782955549438213, 1.509499892929852871 ) ) ;
#17032 = CARTESIAN_POINT ( 'NONE',  ( -2.028188046367890074, 23.41816500000000190, 0.3682158094503220069 ) ) ;
#17033 = CARTESIAN_POINT ( 'NONE',  ( 11.33816213662683658, 22.03852486858766468, 2.072419947804004181 ) ) ;
#17034 = ORIENTED_EDGE ( 'NONE', *, *, #13831, .F. ) ;
#17035 = ORIENTED_EDGE ( 'NONE', *, *, #18833, .T. ) ;
#17036 = AXIS2_PLACEMENT_3D ( 'NONE', #15201, #10099, #16846 ) ;
#17037 = LINE ( 'NONE', #15737, #9533 ) ;
#17038 = CARTESIAN_POINT ( 'NONE',  ( 8.956708553948161011, 11.38351765046557240, 5.092834062626511837 ) ) ;
#17039 = AXIS2_PLACEMENT_3D ( 'NONE', #15667, #20816, #20943 ) ;
#17040 = CARTESIAN_POINT ( 'NONE',  ( 1.396353529130816007, 17.16067149510373469, 8.847120485111785726 ) ) ;
#17041 = CARTESIAN_POINT ( 'NONE',  ( 0.7843704457339527591, -1.594802499999999013, -23.55949434567611078 ) ) ;
#17042 = EDGE_CURVE ( 'NONE', #367, #13909, #6822, .T. ) ;
#17043 = FACE_OUTER_BOUND ( 'NONE', #10912, .T. ) ;
#17044 = VECTOR ( 'NONE', #16076, 1000.000000000000000 ) ;
#17045 = CARTESIAN_POINT ( 'NONE',  ( 12.29981543294080737, 11.04557676861940152, 0.6586324886113450461 ) ) ;
#17046 = DIRECTION ( 'NONE',  ( 0.000000000000000000, 1.000000000000000000, 0.000000000000000000 ) ) ;
#17047 = CARTESIAN_POINT ( 'NONE',  ( 7.524513360980607857, 12.97967409473248246, 7.379558717456829342 ) ) ;
#17048 = DIRECTION ( 'NONE',  ( 1.000000000000000000, 0.000000000000000000, 0.000000000000000000 ) ) ;
#17049 = FACE_OUTER_BOUND ( 'NONE', #20525, .T. ) ;
#17050 = CARTESIAN_POINT ( 'NONE',  ( 1.069455055759913620, 18.50002798056422293, 8.344371670258649232 ) ) ;
#17051 = LINE ( 'NONE', #8415, #21547 ) ;
#17052 = DIRECTION ( 'NONE',  ( 0.000000000000000000, 1.000000000000000000, 0.000000000000000000 ) ) ;
#17053 = CARTESIAN_POINT ( 'NONE',  ( 16.11221013415338632, -8.434765728320028799, -16.05392306811195269 ) ) ;
#17054 = FILL_AREA_STYLE ('',( #13421 ) ) ;
#17055 = FACE_OUTER_BOUND ( 'NONE', #13031, .T. ) ;
#17056 = CARTESIAN_POINT ( 'NONE',  ( 10.50711560308353576, 20.71248852664919227, 5.553285430361647457 ) ) ;
#17057 = EDGE_CURVE ( 'NONE', #10171, #13681, #12625, .T. ) ;
#17058 = CARTESIAN_POINT ( 'NONE',  ( 39.27728671717661513, 0.000000000000000000, -23.95520057284206672 ) ) ;
#17059 = CIRCLE ( 'NONE', #5770, 5.357812499999999645 ) ;
#17060 = VERTEX_POINT ( 'NONE', #16674 ) ;
#17061 = CARTESIAN_POINT ( 'NONE',  ( 11.14798570045502757, 14.97143068324439952, -3.398342535127277575 ) ) ;
#17062 = LINE ( 'NONE', #1798, #11263 ) ;
#17064 = PLANE ( 'NONE',  #20442 ) ;
#17063 = CARTESIAN_POINT ( 'NONE',  ( 3.436982027802252038, 14.00947850804536721, -0.1224347454001346730 ) ) ;
#17065 = ORIENTED_EDGE ( 'NONE', *, *, #15233, .F. ) ;
#17066 = APPLICATION_PROTOCOL_DEFINITION ( 'draft international standard', 'automotive_design', 1998, #14579 ) ;
#17067 = CARTESIAN_POINT ( 'NONE',  ( -7.949728765560771571, -1.265494433638964855, -34.47798802949893826 ) ) ;
#17068 = CARTESIAN_POINT ( 'NONE',  ( 54.84114405289130900, -6.356984999999999886, -18.15059713109360473 ) ) ;
#17069 = EDGE_CURVE ( 'NONE', #3974, #4463, #6877, .T. ) ;
#17070 = CIRCLE ( 'NONE', #20955, 0.7950200000000000600 ) ;
#17071 = ADVANCED_FACE ( 'NONE', ( #19864 ), #4738, .T. ) ;
#17072 = EDGE_CURVE ( 'NONE', #1209, #14379, #9646, .T. ) ;
#17073 = CARTESIAN_POINT ( 'NONE',  ( 6.132461250435506273, 11.01939018619295041, 2.875831410282900791 ) ) ;
#17074 = ORIENTED_EDGE ( 'NONE', *, *, #13424, .T. ) ;
#17075 = CARTESIAN_POINT ( 'NONE',  ( 14.08082576063683966, 20.59196267482642284, 3.841811385045580618 ) ) ;
#17076 = VECTOR ( 'NONE', #10930, 1000.000000000000000 ) ;
#17077 = CARTESIAN_POINT ( 'NONE',  ( 13.53602369538046624, 21.41212481752907948, 2.255110409604365262 ) ) ;
#17078 = CARTESIAN_POINT ( 'NONE',  ( 2.206629122547881572, 16.43321537790008335, -0.5355436742070719403 ) ) ;
#17079 = CARTESIAN_POINT ( 'NONE',  ( 9.343455618504858506, 12.85930032217342145, 6.960085675539649408 ) ) ;
#17080 = CARTESIAN_POINT ( 'NONE',  ( 52.79771328282338771, -1.983739999999999837, 3.317700572842066986 ) ) ;
#17081 = CARTESIAN_POINT ( 'NONE',  ( 17.37611761637614194, 0.7803472578652853597, -15.03203363529809167 ) ) ;
#17082 = LINE ( 'NONE', #6909, #10604 ) ;
#17083 = SHAPE_REPRESENTATION ( 'Ratchet Operating Handle', ( #2234 ), #3303 ) ;
#17084 = EDGE_LOOP ( 'NONE', ( #17972, #17192, #14528, #12151 ) ) ;
#17085 = CARTESIAN_POINT ( 'NONE',  ( 9.164380456484101600, 17.37245550884448875, -3.663273155025991379 ) ) ;
#17086 = VECTOR ( 'NONE', #728, 1000.000000000000000 ) ;
#17087 = EDGE_CURVE ( 'NONE', #4759, #93, #16067, .T. ) ;
#17088 = ORIENTED_EDGE ( 'NONE', *, *, #17057, .T. ) ;
#17089 = CARTESIAN_POINT ( 'NONE',  ( -13.18827588824692754, 32.54247999999999763, -0.8886449702404607409 ) ) ;
#17090 = CARTESIAN_POINT ( 'NONE',  ( 18.07371581377308800, -95.96551800000000298, -11.95909761906105473 ) ) ;
#17092 = LINE ( 'NONE', #16976, #1434 ) ;
#17091 = CARTESIAN_POINT ( 'NONE',  ( 0.08330173461052782502, 11.70670645901422091, 3.276484165168652041 ) ) ;
#17093 = ORIENTED_EDGE ( 'NONE', *, *, #1220, .T. ) ;
#17094 = CARTESIAN_POINT ( 'NONE',  ( 6.663477872564956606, 10.97989248988408129, 3.994247116546560061 ) ) ;
#17095 = AXIS2_PLACEMENT_3D ( 'NONE', #8768, #17185, #14932 ) ;
#17096 = FACE_OUTER_BOUND ( 'NONE', #14291, .T. ) ;
#17097 = ORIENTED_EDGE ( 'NONE', *, *, #9250, .F. ) ;
#17098 = B_SPLINE_CURVE_WITH_KNOTS ( 'NONE', 3,
 ( #17619, #9200, #7559, #7120, #10439, #15767, #816 ),
 .UNSPECIFIED., .F., .F.,
 ( 4, 1, 1, 1, 4 ),
 ( 0.000000000000000000, 0.2500006855674758999, 0.4999999868738881914, 0.7499992881803003719, 1.000000000000000000 ),
 .UNSPECIFIED. ) ;
#17099 = EDGE_CURVE ( 'NONE', #21489, #19201, #834, .T. ) ;
#17100 = CARTESIAN_POINT ( 'NONE',  ( 0.2478183796511415904, 13.05293322038485115, 2.411138524767726832 ) ) ;
#17101 = CYLINDRICAL_SURFACE ( 'NONE', #11786, 0.7950200000000000600 ) ;
#17102 = ORIENTED_EDGE ( 'NONE', *, *, #5715, .F. ) ;
#17103 = CARTESIAN_POINT ( 'NONE',  ( 1.887406236850739827, 14.81135336773366262, 0.3543419383998758221 ) ) ;
#17104 = CIRCLE ( 'NONE', #15725, 0.7950199999999990608 ) ;
#17105 = DIRECTION ( 'NONE',  ( 0.9980811434661737147, 0.000000000000000000, 0.06191955310929838502 ) ) ;
#17106 = CARTESIAN_POINT ( 'NONE',  ( 42.66304184606194383, -9.531985000000000596, -19.22597499813143784 ) ) ;
#17107 = VECTOR ( 'NONE', #20573, 1000.000000000000114 ) ;
#17108 = PRODUCT_DEFINITION_SHAPE ( 'NONE', 'NONE',  #21887 ) ;
#17109 = CARTESIAN_POINT ( 'NONE',  ( -2.234700160307072192, 3.961447500000001565, -24.80708529208898483 ) ) ;
#17110 = CARTESIAN_POINT ( 'NONE',  ( 2.971172838354379397, 21.01571605643849239, 2.270049746313111960 ) ) ;
#17111 = CARTESIAN_POINT ( 'NONE',  ( 7.241402720468077092, 6.343967500000000648, -19.25049230170216319 ) ) ;
#17112 = ORIENTED_EDGE ( 'NONE', *, *, #16068, .T. ) ;
#17113 = FACE_OUTER_BOUND ( 'NONE', #17782, .T. ) ;
#17114 = CARTESIAN_POINT ( 'NONE',  ( 1.291462649553421604, 34.12394749999999988, -20.78637864442907812 ) ) ;
#17115 = PLANE ( 'NONE',  #19431 ) ;
#17116 = ADVANCED_FACE ( 'NONE', ( #16170 ), #14507, .T. ) ;
#17118 = CARTESIAN_POINT ( 'NONE',  ( 15.72888660284841755, -7.237842652465062088, -14.91964761699648889 ) ) ;
#17117 = CARTESIAN_POINT ( 'NONE',  ( -21.73672411175306962, 32.54247999999999763, 0.8886449702404602968 ) ) ;
#17119 = ORIENTED_EDGE ( 'NONE', *, *, #5327, .T. ) ;
#17120 = ADVANCED_FACE ( 'NONE', ( #21640 ), #6501, .T. ) ;
#17121 = EDGE_LOOP ( 'NONE', ( #981, #13175, #11729 ) ) ;
#17122 = EDGE_CURVE ( 'NONE', #1619, #16565, #13687, .T. ) ;
#17123 = CARTESIAN_POINT ( 'NONE',  ( 9.472577224383265104, 12.37763185624888074, -1.056739919939418515 ) ) ;
#17125 = DIRECTION ( 'NONE',  ( 0.000000000000000000, 1.000000000000000000, 0.000000000000000000 ) ) ;
#17124 = CARTESIAN_POINT ( 'NONE',  ( 3.581047328855178069, 13.65542567351872272, -0.8225916644656748877 ) ) ;
#17126 = VERTEX_POINT ( 'NONE', #15354 ) ;
#17127 = CARTESIAN_POINT ( 'NONE',  ( 4.627810217995094177, 11.08939391142007125, 3.992289214736410408 ) ) ;
#17128 = ORIENTED_EDGE ( 'NONE', *, *, #7000, .F. ) ;
#17129 = DIRECTION ( 'NONE',  ( -0.9964481331860212121, 0.000000000000000000, 0.08420877549337305035 ) ) ;
#17130 = ORIENTED_EDGE ( 'NONE', *, *, #19607, .T. ) ;
#17131 = CARTESIAN_POINT ( 'NONE',  ( 7.851649675483148627, 12.13857061077464117, 0.3032157741965843534 ) ) ;
#17132 = CARTESIAN_POINT ( 'NONE',  ( 30.02465935949302533, 39.28268749999999443, -2.324128137548288731 ) ) ;
#17133 = EDGE_LOOP ( 'NONE', ( #7368, #3489, #15788, #5882 ) ) ;
#17134 = CARTESIAN_POINT ( 'NONE',  ( 3.394489146645805810, 14.19730798917363046, 7.892569254303055004 ) ) ;
#17135 = DIRECTION ( 'NONE',  ( 0.000000000000000000, 1.000000000000000000, 0.000000000000000000 ) ) ;
#17136 = DIRECTION ( 'NONE',  ( 0.2490110332224848289, 0.000000000000000000, -0.9685006480810792739 ) ) ;
#17137 = CARTESIAN_POINT ( 'NONE',  ( 2.839491163282604091, 20.06052443223327586, 7.567163413262116833 ) ) ;
#17138 = DIRECTION ( 'NONE',  ( 0.000000000000000000, -1.000000000000000000, -0.000000000000000000 ) ) ;
#17139 = ORIENTED_EDGE ( 'NONE', *, *, #12051, .T. ) ;
#17140 = CARTESIAN_POINT ( 'NONE',  ( 4.620295239943375876, 19.89361395305066083, 0.8378290896073241623 ) ) ;
#17141 = DIRECTION ( 'NONE',  ( 0.9579671649362032637, 0.000000000000000000, -0.2868778675745010664 ) ) ;
#17142 = CARTESIAN_POINT ( 'NONE',  ( 53.10651001381376091, -5.166360000000002728, -16.70269254552787075 ) ) ;
#17143 = DIRECTION ( 'NONE',  ( 0.000000000000000000, -1.000000000000000000, -0.000000000000000000 ) ) ;
#17144 = AXIS2_PLACEMENT_3D ( 'NONE', #20241, #5321, #3457 ) ;
#17145 = VERTEX_POINT ( 'NONE', #403 ) ;
#17146 = EDGE_CURVE ( 'NONE', #16397, #19794, #10358, .T. ) ;
#17147 = CARTESIAN_POINT ( 'NONE',  ( 5.133199192818605816, 13.63276237276972047, -1.377827687522245936 ) ) ;
#17148 = DIRECTION ( 'NONE',  ( 0.000000000000000000, 1.000000000000000000, 0.000000000000000000 ) ) ;
#17149 = CARTESIAN_POINT ( 'NONE',  ( 13.38806052202257035, 14.82377123802367258, 6.981245510777174701 ) ) ;
#17150 = ORIENTED_EDGE ( 'NONE', *, *, #4298, .F. ) ;
#17151 = VERTEX_POINT ( 'NONE', #2045 ) ;
#17152 = PLANE ( 'NONE',  #13096 ) ;
#17153 = CARTESIAN_POINT ( 'NONE',  ( 8.170188656671399485, 10.80366213796246200, 1.764733202284918034 ) ) ;
#17154 = CARTESIAN_POINT ( 'NONE',  ( 7.368554159940218007, 14.94905092387569745, 7.517420915597164743 ) ) ;
#17155 = LINE ( 'NONE', #17041, #19690 ) ;
#17156 = CARTESIAN_POINT ( 'NONE',  ( 6.085205599414213573, 19.08150731743860717, -0.5615252065633009604 ) ) ;
#17157 = CARTESIAN_POINT ( 'NONE',  ( 1.228144954732434124, 20.17113937976969140, 3.320710288574150848 ) ) ;
#17158 = CARTESIAN_POINT ( 'NONE',  ( 29.36874999999999858, 22.62187499999999929, 8.731249999999999289 ) ) ;
#17159 = CARTESIAN_POINT ( 'NONE',  ( 5.973951565552006571, 12.14871438356658295, -0.3439209542975838474 ) ) ;
#17160 = CARTESIAN_POINT ( 'NONE',  ( 46.03750000000000142, 0.000000000000000000, -10.31874999999999964 ) ) ;
#17161 = CARTESIAN_POINT ( 'NONE',  ( 1.758324707547593846, 16.44750854861721834, -0.8283970866775586250 ) ) ;
#17162 = DIRECTION ( 'NONE',  ( 0.9685006480810790519, 0.000000000000000000, 0.2490110332224857170 ) ) ;
#17163 = CARTESIAN_POINT ( 'NONE',  ( 20.16676785488811419, -0.9350613415272122086, -14.77802399055632776 ) ) ;
#17164 = DIRECTION ( 'NONE',  ( -0.9173788132826627972, 0.000000000000000000, 0.3980152169705239440 ) ) ;
#17165 = LINE ( 'NONE', #18, #13635 ) ;
#17166 = CARTESIAN_POINT ( 'NONE',  ( 19.36645978477608310, -7.176659453237705932, -15.34953550627761842 ) ) ;
#17167 = LINE ( 'NONE', #10311, #13 ) ;
#17168 = EDGE_CURVE ( 'NONE', #8930, #6920, #8465, .T. ) ;
#17169 = CARTESIAN_POINT ( 'NONE',  ( 10.40983118653084105, 20.91151375369596366, 5.294894658175683944 ) ) ;
#17170 = CARTESIAN_POINT ( 'NONE',  ( 61.02111788801703085, 34.52875999999999834, -5.406220493519755088 ) ) ;
#17171 = CARTESIAN_POINT ( 'NONE',  ( 11.33353759921747539, 17.80752733036843694, -3.397307814249996394 ) ) ;
#17172 = CARTESIAN_POINT ( 'NONE',  ( 19.95643545564609056, -1.593178449655435092, -15.48935439063656538 ) ) ;
#17174 = DIRECTION ( 'NONE',  ( 0.2868778675745004558, 0.000000000000000000, 0.9579671649362035968 ) ) ;
#17173 = CARTESIAN_POINT ( 'NONE',  ( 2.556459638088360187, 19.27890597942106155, 7.589709452800516232 ) ) ;
#17175 = VERTEX_POINT ( 'NONE', #18963 ) ;
#17176 = APPLICATION_PROTOCOL_DEFINITION ( 'draft international standard', 'automotive_design', 1998, #13024 ) ;
#17177 =( NAMED_UNIT ( * ) PLANE_ANGLE_UNIT ( ) SI_UNIT ( $, .RADIAN. ) );
#17178 = CARTESIAN_POINT ( 'NONE',  ( 29.15193331460030279, 30.55334249999999940, -13.61707959051006966 ) ) ;
#17179 = PLANE ( 'NONE',  #17470 ) ;
#17180 = CARTESIAN_POINT ( 'NONE',  ( 20.48137360697176490, -5.937212919150582913, -14.37931843660670062 ) ) ;
#17181 = ORIENTED_EDGE ( 'NONE', *, *, #7225, .T. ) ;
#17182 = CARTESIAN_POINT ( 'NONE',  ( 6.208034055486434610, 11.87704527764502060, 1.587409285954058058 ) ) ;
#17183 = CARTESIAN_POINT ( 'NONE',  ( 11.10955948574564900, 17.51362067755397334, 6.777590957738523159 ) ) ;
#17184 = CARTESIAN_POINT ( 'NONE',  ( 8.134723707567005135, 10.68876677029517985, 1.740177802357664616 ) ) ;
#17185 = DIRECTION ( 'NONE',  ( 0.000000000000000000, 1.000000000000000000, 0.000000000000000000 ) ) ;
#17186 = CARTESIAN_POINT ( 'NONE',  ( 14.25471133999911011, 0.7535054429800847053, -15.99185436641439217 ) ) ;
#17187 = CARTESIAN_POINT ( 'NONE',  ( 30.42699695299585017, 36.51313500000000545, -4.832012189960551041 ) ) ;
#17188 = ADVANCED_FACE ( 'NONE', ( #15242 ), #17101, .F. ) ;
#17189 = VERTEX_POINT ( 'NONE', #8909 ) ;
#17190 = EDGE_CURVE ( 'NONE', #7998, #2524, #5053, .T. ) ;
#17191 = CARTESIAN_POINT ( 'NONE',  ( 6.928309554343074161, 11.28692669747560018, 5.045805056684474543 ) ) ;
#17192 = ORIENTED_EDGE ( 'NONE', *, *, #19993, .F. ) ;
#17193 = CARTESIAN_POINT ( 'NONE',  ( 10.20496955028552577, 11.36774521743359223, 1.751886196687873598 ) ) ;
#17194 = CARTESIAN_POINT ( 'NONE',  ( -17.46249999999999858, -0.3962399999999990929, 0.000000000000000000 ) ) ;
#17195 = DIRECTION ( 'NONE',  ( 0.000000000000000000, 1.000000000000000000, 0.000000000000000000 ) ) ;
#17197 = CYLINDRICAL_SURFACE ( 'NONE', #1793, 0.5953124999999994671 ) ;
#17196 = CARTESIAN_POINT ( 'NONE',  ( 7.251559452448354648, 14.74276822600529258, 8.275638029269909879 ) ) ;
#17198 = ORIENTED_EDGE ( 'NONE', *, *, #4494, .T. ) ;
#17199 = CARTESIAN_POINT ( 'NONE',  ( 7.403462572312458967, 13.02891555264111112, 7.298645462994318045 ) ) ;
#17200 = FACE_OUTER_BOUND ( 'NONE', #11442, .T. ) ;
#17201 = ORIENTED_EDGE ( 'NONE', *, *, #14790, .T. ) ;
#17202 = CIRCLE ( 'NONE', #21794, 9.524999999999998579 ) ;
#17203 = CARTESIAN_POINT ( 'NONE',  ( 12.02474915109715603, -95.96551800000000298, -13.51434638588835391 ) ) ;
#17204 = ORIENTED_EDGE ( 'NONE', *, *, #17650, .F. ) ;
#17205 = CARTESIAN_POINT ( 'NONE',  ( 2.133183598781188905, 12.85820387514107033, 1.817181390205857561 ) ) ;
#17206 = EDGE_CURVE ( 'NONE', #6814, #3875, #5253, .T. ) ;
#17207 = ADVANCED_BREP_SHAPE_REPRESENTATION ( '', ( #21013, #2234 ), #14439 ) ;
#17208 = FACE_OUTER_BOUND ( 'NONE', #5395, .T. ) ;
#17209 = CARTESIAN_POINT ( 'NONE',  ( -17.46249999999999858, 32.54247999999999763, 0.000000000000000000 ) ) ;
#17210 = DIRECTION ( 'NONE',  ( 0.000000000000000000, 1.000000000000000000, -0.000000000000000000 ) ) ;
#17211 = CARTESIAN_POINT ( 'NONE',  ( 4.091290149016956867, 21.18971284961126145, 5.301660524291831322 ) ) ;
#17212 = DIRECTION ( 'NONE',  ( 0.000000000000000000, 1.000000000000000000, 0.000000000000000000 ) ) ;
#17213 = ORIENTED_EDGE ( 'NONE', *, *, #20412, .F. ) ;
#17214 = EDGE_CURVE ( 'NONE', #21739, #7796, #14636, .T. ) ;
#17215 = CARTESIAN_POINT ( 'NONE',  ( 43.29176983217143260, 34.52875999999999834, 5.154088326438659884 ) ) ;
#17216 = CARTESIAN_POINT ( 'NONE',  ( 1.173720826352361080, 34.12394749999999988, -20.82884779549221577 ) ) ;
#17217 = FACE_OUTER_BOUND ( 'NONE', #4229, .T. ) ;
#17218 = FACE_OUTER_BOUND ( 'NONE', #16897, .T. ) ;
#17220 = CARTESIAN_POINT ( 'NONE',  ( 18.21294863246763640, -6.358645335814493649, -14.40912211738714888 ) ) ;
#17219 = LINE ( 'NONE', #8697, #21493 ) ;
#17221 = EDGE_LOOP ( 'NONE', ( #19612, #6541, #17740, #12137 ) ) ;
#17222 = ORIENTED_EDGE ( 'NONE', *, *, #4379, .T. ) ;
#17223 = CARTESIAN_POINT ( 'NONE',  ( 11.21039383726165184, 12.85296284657052190, -2.355313754033094398 ) ) ;
#17224 = CARTESIAN_POINT ( 'NONE',  ( 2.307410737991283600, 19.81104553907935895, 0.4478696585410927855 ) ) ;
#17225 = VERTEX_POINT ( 'NONE', #13468 ) ;
#17227 = CARTESIAN_POINT ( 'NONE',  ( 17.24715906500612306, 2.440694956846978680, -14.94721736399773704 ) ) ;
#17226 = CARTESIAN_POINT ( 'NONE',  ( 5.537219767437146167, 13.75671170515803077, 8.140707804000232528 ) ) ;
#17228 = EDGE_CURVE ( 'NONE', #107, #1117, #2251, .T. ) ;
#17229 = VERTEX_POINT ( 'NONE', #11905 ) ;
#17230 = ORIENTED_EDGE ( 'NONE', *, *, #13040, .T. ) ;
#17231 = APPLICATION_CONTEXT ( 'automotive_design' ) ;
#17232 = CARTESIAN_POINT ( 'NONE',  ( 7.838781466353688110, 18.78645029527194410, -1.510171260141905281 ) ) ;
#17233 = DIRECTION ( 'NONE',  ( -0.2868778675745011220, 0.000000000000000000, -0.9579671649362034858 ) ) ;
#17234 = ORIENTED_EDGE ( 'NONE', *, *, #11200, .T. ) ;
#17235 = CARTESIAN_POINT ( 'NONE',  ( 3.332431224701041916, 13.62386199439126599, 7.503246970460915044 ) ) ;
#17236 = EDGE_CURVE ( 'NONE', #16695, #19840, #10013, .T. ) ;
#17237 = EDGE_CURVE ( 'NONE', #14357, #12696, #21308, .T. ) ;
#17238 = ADVANCED_FACE ( 'NONE', ( #2166 ), #12013, .F. ) ;
#17239 = CARTESIAN_POINT ( 'NONE',  ( -22.90596259062238005, -6.905625000000000568, -9.869321627248080375 ) ) ;
#17240 = DIRECTION ( 'NONE',  ( -0.3447671952293630548, 0.000000000000000000, -0.9386882235831439658 ) ) ;
#17241 = DIRECTION ( 'NONE',  ( 0.000000000000000000, 1.000000000000000000, 0.000000000000000000 ) ) ;
#17242 = DIRECTION ( 'NONE',  ( -0.7532174416907910786, 0.000000000000000000, -0.6577716059034319773 ) ) ;
#17243 = CARTESIAN_POINT ( 'NONE',  ( 3.485229903966501563, 17.58310126945597673, 9.057586764078154218 ) ) ;
#17244 = CARTESIAN_POINT ( 'NONE',  ( 23.49608546833631451, 3.565842500000000914, -17.12016812500874252 ) ) ;
#17245 = ORIENTED_EDGE ( 'NONE', *, *, #14166, .F. ) ;
#17246 = PRODUCT_DEFINITION_FORMATION_WITH_SPECIFIED_SOURCE ( 'ANY', '', #17286, .NOT_KNOWN. ) ;
#17247 = CARTESIAN_POINT ( 'NONE',  ( 7.384935211504371821, 18.21544151669790068, 7.341947698684717416 ) ) ;
#17248 = DIRECTION ( 'NONE',  ( -0.3928209820863022839, 0.000000000000000000, 0.9196149607486564515 ) ) ;
#17249 = CARTESIAN_POINT ( 'NONE',  ( 52.43369301778259484, -7.088958102700910757, -17.37753678331790397 ) ) ;
#17250 = ORIENTED_EDGE ( 'NONE', *, *, #570, .T. ) ;
#17251 = CARTESIAN_POINT ( 'NONE',  ( 11.02290331352381791, 22.07868470824458385, 2.113619312756540136 ) ) ;
#17252 = CYLINDRICAL_SURFACE ( 'NONE', #12068, 1.785937499999999512 ) ;
#17253 = CARTESIAN_POINT ( 'NONE',  ( 11.42651139047453768, 22.02362793052084200, 2.317792814824360725 ) ) ;
#17254 = VERTEX_POINT ( 'NONE', #12238 ) ;
#17255 = ORIENTED_EDGE ( 'NONE', *, *, #4953, .F. ) ;
#17256 = CARTESIAN_POINT ( 'NONE',  ( 12.95548479057611502, 21.40508096933954363, 0.7262709874220900641 ) ) ;
#17257 = VECTOR ( 'NONE', #6863, 1000.000000000000114 ) ;
#17258 = CARTESIAN_POINT ( 'NONE',  ( 9.385496763270603893, 17.22841133438524608, 7.914895363721495158 ) ) ;
#17259 = CARTESIAN_POINT ( 'NONE',  ( 1.919263925057361542, 16.41907190720915466, -0.02685608345594442739 ) ) ;
#17260 = DIRECTION ( 'NONE',  ( 0.7334850928793773539, -0.6768732144311023768, -0.06198604769976947398 ) ) ;
#17261 = CARTESIAN_POINT ( 'NONE',  ( 5.618432726368788543, 16.25838397047299111, -1.398541098735894606 ) ) ;
#17262 = CARTESIAN_POINT ( 'NONE',  ( 7.263313943976001497, 16.57996653523900932, 7.625354271785694138 ) ) ;
#17263 = DIRECTION ( 'NONE',  ( 0.000000000000000000, 1.000000000000000000, 0.000000000000000000 ) ) ;
#17264 = EDGE_CURVE ( 'NONE', #3845, #18633, #20501, .T. ) ;
#17265 = CARTESIAN_POINT ( 'NONE',  ( 9.340232214130086419, 11.57391542797248007, 5.373554129697876824 ) ) ;
#17266 = DIRECTION ( 'NONE',  ( 0.000000000000000000, -1.000000000000000000, 0.000000000000000000 ) ) ;
#17267 = CARTESIAN_POINT ( 'NONE',  ( 2.985887990111508739, 19.78048590522542227, 8.004448071915154728 ) ) ;
#17268 = CARTESIAN_POINT ( 'NONE',  ( 0.2766951009951102436, 20.85331682198317438, 6.385187645444293736 ) ) ;
#17269 = CIRCLE ( 'NONE', #8433, 3.175000000000000711 ) ;
#17270 = CARTESIAN_POINT ( 'NONE',  ( 20.18678758757129543, -1.006362617683279836, -14.77198301169015693 ) ) ;
#17271 = CARTESIAN_POINT ( 'NONE',  ( 2.818516750425272388, 19.21826933052950181, 7.445547682248660593 ) ) ;
#17272 = DIRECTION ( 'NONE',  ( 0.08420877549337300871, 0.000000000000000000, 0.9964481331860212121 ) ) ;
#17273 = LINE ( 'NONE', #8416, #20305 ) ;
#17274 = CARTESIAN_POINT ( 'NONE',  ( 16.07189111700614603, 2.286673086399800159, -15.43580752111316556 ) ) ;
#17275 = CYLINDRICAL_SURFACE ( 'NONE', #17347, 3.968750000000001776 ) ;
#17276 = VECTOR ( 'NONE', #3825, 1000.000000000000000 ) ;
#17277 = FACE_OUTER_BOUND ( 'NONE', #8902, .T. ) ;
#17278 = CARTESIAN_POINT ( 'NONE',  ( 9.775410964689198678, 21.72172014376007354, 3.570919871311593052 ) ) ;
#17279 = VECTOR ( 'NONE', #3345, 1000.000000000000114 ) ;
#17280 = LINE ( 'NONE', #2125, #19104 ) ;
#17281 = CARTESIAN_POINT ( 'NONE',  ( 11.24486007184577829, 13.45202003486185127, -2.714015282924980177 ) ) ;
#17282 = CARTESIAN_POINT ( 'NONE',  ( 12.53323336751100392, -6.117360363457603256, -15.61470599677969595 ) ) ;
#17283 = ORIENTED_EDGE ( 'NONE', *, *, #13454, .T. ) ;
#17284 = CARTESIAN_POINT ( 'NONE',  ( 9.137394532338957376, -14.84248999999999974, -13.43583653331040750 ) ) ;
#17285 = DIRECTION ( 'NONE',  ( 0.000000000000000000, -1.000000000000000000, -0.000000000000000000 ) ) ;
#17286 = PRODUCT ( 'Split Webbing Winding Axle', 'Split Webbing Winding Axle', '', ( #12434 ) ) ;
#17287 = EDGE_CURVE ( 'NONE', #15983, #6204, #20282, .T. ) ;
#17288 = CARTESIAN_POINT ( 'NONE',  ( 14.61877701993662981, -8.672575780289569991, -15.30737042585371377 ) ) ;
#17289 = ORIENTED_EDGE ( 'NONE', *, *, #10148, .T. ) ;
#17290 = CARTESIAN_POINT ( 'NONE',  ( 9.332179563246018716, 16.57955862325433571, 7.285397067016122996 ) ) ;
#17291 = AXIS2_PLACEMENT_3D ( 'NONE', #5015, #8105, #11770 ) ;
#17292 = AXIS2_PLACEMENT_3D ( 'NONE', #15304, #18915, #17046 ) ;
#17293 = CARTESIAN_POINT ( 'NONE',  ( 12.89786562617043586, 21.48375758380098333, 0.4863175907518038077 ) ) ;
#17294 = CARTESIAN_POINT ( 'NONE',  ( 0.2312783866436057267, 17.35729252269350553, 0.02433704674567344767 ) ) ;
#17295 = CARTESIAN_POINT ( 'NONE',  ( 26.59920545652001067, 3.961447500000001565, -43.69048495915765074 ) ) ;
#17296 = CARTESIAN_POINT ( 'NONE',  ( 53.13667458378568398, -7.546788837613773282, -16.66913787414813086 ) ) ;
#17297 = CARTESIAN_POINT ( 'NONE',  ( 19.40549191052905798, -1.213055114509968613, -14.37046020240782518 ) ) ;
#17298 = DIRECTION ( 'NONE',  ( 0.5087559856598092844, 0.000000000000000000, 0.8609107660235849613 ) ) ;
#17299 = AXIS2_PLACEMENT_3D ( 'NONE', #8008, #1161, #11219 ) ;
#17300 = VERTEX_POINT ( 'NONE', #18634 ) ;
#17301 = CARTESIAN_POINT ( 'NONE',  ( 5.427037647511713025, 13.59023913265000338, -1.545513002505085165 ) ) ;
#17302 = FACE_OUTER_BOUND ( 'NONE', #1862, .T. ) ;
#17303 = ORIENTED_EDGE ( 'NONE', *, *, #16529, .F. ) ;
#17304 = CARTESIAN_POINT ( 'NONE',  ( 9.383108080252510419, 13.57643509814862526, -2.023504206776891134 ) ) ;
#17305 = DIRECTION ( 'NONE',  ( 0.000000000000000000, 1.000000000000000000, 0.000000000000000000 ) ) ;
#17306 = CARTESIAN_POINT ( 'NONE',  ( 12.85172960207861337, 22.16157334387418842, 0.4256939560979881021 ) ) ;
#17307 = CIRCLE ( 'NONE', #13439, 30.16249999999999432 ) ;
#17309 = FACE_OUTER_BOUND ( 'NONE', #20662, .T. ) ;
#17308 = CARTESIAN_POINT ( 'NONE',  ( -0.06148638314567612950, 18.97471059823722328, 0.8203174876396049919 ) ) ;
#17310 = ORIENTED_EDGE ( 'NONE', *, *, #1816, .F. ) ;
#17311 = CARTESIAN_POINT ( 'NONE',  ( 7.334099821040434009, 12.60367174608902729, 6.953311051513514585 ) ) ;
#17312 = AXIS2_PLACEMENT_3D ( 'NONE', #4255, #12327, #15779 ) ;
#17313 = CARTESIAN_POINT ( 'NONE',  ( -17.01419847615277092, -1.983739999999999393, -25.90052557009608236 ) ) ;
#17314 = ORIENTED_EDGE ( 'NONE', *, *, #20823, .F. ) ;
#17315 = CARTESIAN_POINT ( 'NONE',  ( 49.28028498622276032, -1.983739999999999837, -25.68670502218146368 ) ) ;
#17316 = CARTESIAN_POINT ( 'NONE',  ( 0.1102113429977584769, 16.78173416929226391, 0.8122148397512033435 ) ) ;
#17317 = EDGE_CURVE ( 'NONE', #11827, #7489, #18534, .T. ) ;
#17318 = DIRECTION ( 'NONE',  ( 0.000000000000000000, 1.000000000000000000, 0.000000000000000000 ) ) ;
#17319 = VERTEX_POINT ( 'NONE', #5371 ) ;
#17320 = DIRECTION ( 'NONE',  ( 0.2490110332224848289, 0.000000000000000000, -0.9685006480810792739 ) ) ;
#17321 = CARTESIAN_POINT ( 'NONE',  ( 1.884251155305252112, 15.59442180266581701, 0.1340261972781983113 ) ) ;
#17322 = VECTOR ( 'NONE', #3501, 1000.000000000000114 ) ;
#17323 = CARTESIAN_POINT ( 'NONE',  ( 29.76562500000000000, 32.54502000000000095, -4.317999999999999616 ) ) ;
#17324 = DIRECTION ( 'NONE',  ( 0.5087559856598092844, 0.000000000000000000, 0.8609107660235849613 ) ) ;
#17325 = AXIS2_PLACEMENT_3D ( 'NONE', #4803, #19606, #16424 ) ;
#17326 = CARTESIAN_POINT ( 'NONE',  ( 28.87608719841374949, -7.547927499999999235, -15.73691681567849976 ) ) ;
#17327 = LINE ( 'NONE', #8916, #5535 ) ;
#17328 = ORIENTED_EDGE ( 'NONE', *, *, #7217, .F. ) ;
#17329 = CARTESIAN_POINT ( 'NONE',  ( 55.81697695389291169, 34.52875999999999834, -11.14520323105768362 ) ) ;
#17330 = CARTESIAN_POINT ( 'NONE',  ( -14.39647200192766441, 34.52875999999985623, -9.747027169376242028 ) ) ;
#17331 = DIRECTION ( 'NONE',  ( -1.000000000000000000, 0.000000000000000000, 0.000000000000000000 ) ) ;
#17333 = CARTESIAN_POINT ( 'NONE',  ( 12.58984874085997419, -5.789910881123263131, -15.55645878085723233 ) ) ;
#17332 = DIRECTION ( 'NONE',  ( 1.000000000000000000, 0.000000000000000000, 0.000000000000000000 ) ) ;
#17334 = VECTOR ( 'NONE', #8161, 1000.000000000000000 ) ;
#17335 = VERTEX_POINT ( 'NONE', #10133 ) ;
#17336 = ORIENTED_EDGE ( 'NONE', *, *, #6781, .T. ) ;
#17337 = CARTESIAN_POINT ( 'NONE',  ( 14.01635924107887199, 20.58788406416984174, 3.858321978819213349 ) ) ;
#17338 = AXIS2_PLACEMENT_3D ( 'NONE', #11274, #2881, #9612 ) ;
#17340 = DIRECTION ( 'NONE',  ( -0.9964481331860212121, 0.000000000000000000, 0.08420877549337300871 ) ) ;
#17339 = CARTESIAN_POINT ( 'NONE',  ( 0.2423679456950503242, 19.02238102577908307, 0.6537417863645457183 ) ) ;
#17341 = ORIENTED_EDGE ( 'NONE', *, *, #13023, .T. ) ;
#17343 = CARTESIAN_POINT ( 'NONE',  ( 10.34597555076318187, -3.120040139117916222, -17.08279145937373045 ) ) ;
#17342 = CARTESIAN_POINT ( 'NONE',  ( 4.483212079453008592, 11.09257280940468071, 3.375105758503219811 ) ) ;
#17344 = EDGE_CURVE ( 'NONE', #13849, #12892, #11330, .T. ) ;
#17345 = ORIENTED_EDGE ( 'NONE', *, *, #764, .T. ) ;
#17346 = ORIENTED_EDGE ( 'NONE', *, *, #12382, .T. ) ;
#17347 = AXIS2_PLACEMENT_3D ( 'NONE', #11973, #1789, #8648 ) ;
#17348 = CARTESIAN_POINT ( 'NONE',  ( 7.940458870083464404, 19.15559514504086280, -1.273737374462845295 ) ) ;
#17349 = CARTESIAN_POINT ( 'NONE',  ( 1.479369755814697651, 14.83370841331159973, 8.578845862358663865 ) ) ;
#17350 = ADVANCED_FACE ( 'NONE', ( #12136, #12801 ), #7909, .T. ) ;
#17351 = EDGE_LOOP ( 'NONE', ( #21053, #3989, #9706, #15148 ) ) ;
#17352 = ADVANCED_FACE ( 'NONE', ( #4175 ), #6261, .T. ) ;
#17353 = VECTOR ( 'NONE', #4817, 1000.000000000000000 ) ;
#17354 = AXIS2_PLACEMENT_3D ( 'NONE', #11465, #11567, #18305 ) ;
#17355 = AXIS2_PLACEMENT_3D ( 'NONE', #15536, #10435, #17174 ) ;
#17356 = CARTESIAN_POINT ( 'NONE',  ( 29.22749461619170219, 2.019535839764540430, -4.986088976786413163 ) ) ;
#17357 = CARTESIAN_POINT ( 'NONE',  ( 38.27575909311416780, -6.969031819622845347, -4.797431545001941799 ) ) ;
#17358 = CARTESIAN_POINT ( 'NONE',  ( 20.76310168089343478, -3.968114999999999615, -11.26763008640078212 ) ) ;
#17359 = CARTESIAN_POINT ( 'NONE',  ( 2.447168770603926458, 20.74837111547305213, 6.544952949461906755 ) ) ;
#17360 = CIRCLE ( 'NONE', #19821, 0.7950200000000005041 ) ;
#17361 = DIRECTION ( 'NONE',  ( -0.000000000000000000, 1.000000000000000000, 0.000000000000000000 ) ) ;
#17362 = VERTEX_POINT ( 'NONE', #8028 ) ;
#17363 = CARTESIAN_POINT ( 'NONE',  ( 3.716496455301536717, 18.12196835462199829, 8.451690309147281255 ) ) ;
#17364 = CARTESIAN_POINT ( 'NONE',  ( 11.85370378511233191, -4.423560566297380703, -15.83226420197127204 ) ) ;
#17365 = DIRECTION ( 'NONE',  ( -0.5087559856598089514, 0.000000000000000000, -0.8609107660235851833 ) ) ;
#17366 = VECTOR ( 'NONE', #3013, 1000.000000000000000 ) ;
#17367 = VERTEX_POINT ( 'NONE', #21513 ) ;
#17368 = ORIENTED_EDGE ( 'NONE', *, *, #15516, .T. ) ;
#17369 = CARTESIAN_POINT ( 'NONE',  ( 5.313704621423529062, 12.39088710148332062, 0.06850381583308091937 ) ) ;
#17370 = DIRECTION ( 'NONE',  ( 1.000000000000000000, 0.000000000000000000, 0.000000000000000000 ) ) ;
#17371 = CARTESIAN_POINT ( 'NONE',  ( 12.72335754809818553, 10.91377108077479186, 3.768601682827632970 ) ) ;
#17372 = ORIENTED_EDGE ( 'NONE', *, *, #21331, .F. ) ;
#17373 = ADVANCED_FACE ( 'NONE', ( #860 ), #14468, .T. ) ;
#17374 = AXIS2_PLACEMENT_3D ( 'NONE', #2354, #690, #2010 ) ;
#17375 = ORIENTED_EDGE ( 'NONE', *, *, #16277, .T. ) ;
#17376 = DIRECTION ( 'NONE',  ( 0.000000000000000000, -1.000000000000000000, 0.000000000000000000 ) ) ;
#17377 = TOROIDAL_SURFACE ( 'NONE', #4651, 3.174999999999999822, 1.190625000000000044 ) ;
#17378 = PRODUCT_DEFINITION ( 'UNKNOWN', '', #11248, #10993 ) ;
#17379 = CARTESIAN_POINT ( 'NONE',  ( 7.558441812221111000, 18.80437392093399396, -2.356808005286376240 ) ) ;
#17380 = CARTESIAN_POINT ( 'NONE',  ( 4.555732288980417266, 19.89758433537658178, 0.8540176713598968128 ) ) ;
#17381 = DIRECTION ( 'NONE',  ( 0.000000000000000000, 1.000000000000000000, 0.000000000000000000 ) ) ;
#17382 = CARTESIAN_POINT ( 'NONE',  ( 6.008477055667284183, 18.80194823471332910, -0.7371998150550872486 ) ) ;
#17383 = AXIS2_PLACEMENT_3D ( 'NONE', #1417, #4750, #18328 ) ;
#17384 = VECTOR ( 'NONE', #7061, 999.9999999999998863 ) ;
#17385 = CARTESIAN_POINT ( 'NONE',  ( 1.580519713932151182, 20.39156962568002029, 4.231171962872529946 ) ) ;
#17386 = CARTESIAN_POINT ( 'NONE',  ( 38.96848998618624904, 37.69740999999999786, -3.934807454472129429 ) ) ;
#17387 = FACE_BOUND ( 'NONE', #6633, .T. ) ;
#17388 = CARTESIAN_POINT ( 'NONE',  ( 11.97441025620787514, 11.34274383772578254, -1.271560673672284869 ) ) ;
#17389 = CIRCLE ( 'NONE', #18083, 1.190625000000000711 ) ;
#17390 = LINE ( 'NONE', #2230, #18499 ) ;
#17391 = CARTESIAN_POINT ( 'NONE',  ( 1.219148700260345164, 21.11368951514764092, 3.320743722783168650 ) ) ;
#17392 = CARTESIAN_POINT ( 'NONE',  ( 1.350832016589100570, 18.54689706714595232, 9.095633459574033353 ) ) ;
#17393 = CIRCLE ( 'NONE', #781, 0.5080000000000016724 ) ;
#17394 = FACE_OUTER_BOUND ( 'NONE', #11829, .T. ) ;
#17395 = CARTESIAN_POINT ( 'NONE',  ( 3.729879025887206989, 14.05198016149147122, -0.1312770743009889218 ) ) ;
#17396 = CARTESIAN_POINT ( 'NONE',  ( 30.78626241496060700, -5.959792500000001603, -2.552201779827368622 ) ) ;
#17397 = CARTESIAN_POINT ( 'NONE',  ( 64.19677489640052670, 29.95901653600000003, -11.74367670905533423 ) ) ;
#17398 = CARTESIAN_POINT ( 'NONE',  ( 15.49294960918546238, 2.279643855968550792, -15.60671101686425288 ) ) ;
#17399 = CARTESIAN_POINT ( 'NONE',  ( -1.848761088705630051, 9.129395000000000593, 7.884515871828260636 ) ) ;
#17400 = VECTOR ( 'NONE', #12893, 1000.000000000000000 ) ;
#17401 = CARTESIAN_POINT ( 'NONE',  ( 10.62170397221806084, 10.78185011543068228, 3.503052559935591059 ) ) ;
#17402 = ORIENTED_EDGE ( 'NONE', *, *, #5899, .F. ) ;
#17403 = EDGE_CURVE ( 'NONE', #5334, #2409, #10165, .T. ) ;
#17404 = CARTESIAN_POINT ( 'NONE',  ( 57.69402548289047417, 0.000000000000000000, -20.84562559047711261 ) ) ;
#17405 = EDGE_CURVE ( 'NONE', #18990, #12688, #17988, .T. ) ;
#17406 = CARTESIAN_POINT ( 'NONE',  ( 11.62317935382189660, 11.79670150420027674, -0.9113138770421064239 ) ) ;
#17407 = CARTESIAN_POINT ( 'NONE',  ( 19.52837946232106248, -0.8676311488457835175, -15.63954645954029843 ) ) ;
#17408 = VERTEX_POINT ( 'NONE', #6043 ) ;
#17409 =( LENGTH_UNIT ( ) NAMED_UNIT ( * ) SI_UNIT ( .MILLI., .METRE. ) );
#17410 = AXIS2_PLACEMENT_3D ( 'NONE', #16421, #9981, #8318 ) ;
#17411 = DIRECTION ( 'NONE',  ( -0.9964481331860212121, 0.000000000000000000, 0.08420877549337302259 ) ) ;
#17412 = VECTOR ( 'NONE', #20097, 1000.000000000000000 ) ;
#17413 = ORIENTED_EDGE ( 'NONE', *, *, #11325, .F. ) ;
#17414 = AXIS2_PLACEMENT_3D ( 'NONE', #7777, #3030, #2700 ) ;
#17415 = CARTESIAN_POINT ( 'NONE',  ( 10.39407546256930281, 11.26810435610842198, 2.151588622715834731 ) ) ;
#17416 = CARTESIAN_POINT ( 'NONE',  ( 11.11863957019668803, 17.51379554528373816, 6.775575702281829926 ) ) ;
#17417 = FACE_OUTER_BOUND ( 'NONE', #2639, .T. ) ;
#17418 = DIRECTION ( 'NONE',  ( 0.000000000000000000, -1.000000000000000000, -0.000000000000000000 ) ) ;
#17419 = CIRCLE ( 'NONE', #5752, 0.3962399999999980382 ) ;
#17420 = CARTESIAN_POINT ( 'NONE',  ( 12.41531557771041783, -0.9351939426588545823, -16.58710729350898561 ) ) ;
#17421 = DIRECTION ( 'NONE',  ( -0.8192319205190408127, 0.5734623443633278805, 0.000000000000000000 ) ) ;
#17422 = VERTEX_POINT ( 'NONE', #12814 ) ;
#17423 = CARTESIAN_POINT ( 'NONE',  ( 5.677614812627209240, 12.08210925389420076, -0.3142286978463815217 ) ) ;
#17424 = CYLINDRICAL_SURFACE ( 'NONE', #10926, 0.5080000000000001181 ) ;
#17425 = ORIENTED_EDGE ( 'NONE', *, *, #18599, .T. ) ;
#17426 = EDGE_CURVE ( 'NONE', #13109, #21133, #2843, .T. ) ;
#17427 = CARTESIAN_POINT ( 'NONE',  ( 9.337275534366419549, 14.04566788780411635, -2.298141133598044394 ) ) ;
#17428 = CARTESIAN_POINT ( 'NONE',  ( 46.03750000000000142, 36.51313500000000545, -10.31874999999999964 ) ) ;
#17429 = CIRCLE ( 'NONE', #12851, 0.5080000000000012284 ) ;
#17430 = CARTESIAN_POINT ( 'NONE',  ( 29.76562500000000000, 32.54502000000000095, -4.317999999999999616 ) ) ;
#17432 = CARTESIAN_POINT ( 'NONE',  ( 49.72033008250774344, -1.983739999999999837, -2.687827786179598277 ) ) ;
#17431 = CARTESIAN_POINT ( 'NONE',  ( -1.102394795307540809, 20.42992192302084220, 3.974520701941598233 ) ) ;
#17433 = ORIENTED_EDGE ( 'NONE', *, *, #14248, .T. ) ;
#17434 = CARTESIAN_POINT ( 'NONE',  ( 7.537868633733004309, 14.58841703367216169, 8.112932634158456224 ) ) ;
#17435 = PLANE ( 'NONE',  #21459 ) ;
#17436 = EDGE_LOOP ( 'NONE', ( #4490, #15154, #12846, #4322 ) ) ;
#17437 = CARTESIAN_POINT ( 'NONE',  ( 19.42680641351661919, 0.4165720343021085958, -14.98010323326712268 ) ) ;
#17438 = CARTESIAN_POINT ( 'NONE',  ( 0.05952623492205127986, 14.33507843624741085, 1.323949193066850771 ) ) ;
#17439 = CIRCLE ( 'NONE', #13206, 1.785937499999998179 ) ;
#17440 = CARTESIAN_POINT ( 'NONE',  ( 12.43890308457113747, -5.664764769703692693, -16.75625553099141385 ) ) ;
#17441 = ORIENTED_EDGE ( 'NONE', *, *, #19305, .T. ) ;
#17442 = CARTESIAN_POINT ( 'NONE',  ( 17.34610635302146164, 13.08957250000000094, -18.70138818597152053 ) ) ;
#17443 = LINE ( 'NONE', #9025, #8547 ) ;
#17444 = CARTESIAN_POINT ( 'NONE',  ( 1.538729348984987588, 9.085401985160794780, 10.69440411747507724 ) ) ;
#17445 = ORIENTED_EDGE ( 'NONE', *, *, #12328, .F. ) ;
#17446 = CYLINDRICAL_SURFACE ( 'NONE', #1867, 0.5079999999999984528 ) ;
#17447 = CARTESIAN_POINT ( 'NONE',  ( 55.52866846859685523, -14.84248999999999974, -11.12083858657437752 ) ) ;
#17448 = DIRECTION ( 'NONE',  ( 0.000000000000000000, 1.000000000000000000, 0.000000000000000000 ) ) ;
#17449 = AXIS2_PLACEMENT_3D ( 'NONE', #8854, #19020, #7097 ) ;
#17450 = ORIENTED_EDGE ( 'NONE', *, *, #8716, .T. ) ;
#17451 = VERTEX_POINT ( 'NONE', #14589 ) ;
#17452 = ADVANCED_FACE ( 'NONE', ( #21298 ), #12925, .F. ) ;
#17454 = CARTESIAN_POINT ( 'NONE',  ( 17.30373842852263877, -3.968114999999999615, -12.15706637069277107 ) ) ;
#17453 = CARTESIAN_POINT ( 'NONE',  ( 3.450391172034505960, 21.44980502101282127, 3.507873031676746578 ) ) ;
#17455 = ORIENTED_EDGE ( 'NONE', *, *, #12764, .T. ) ;
#17457 = CARTESIAN_POINT ( 'NONE',  ( 20.48685332741090903, -6.007402871720267434, -13.93096415391416976 ) ) ;
#17456 = CARTESIAN_POINT ( 'NONE',  ( 5.596169840114256111, 14.78911034132691427, 8.577020563439660350 ) ) ;
#17458 = ORIENTED_EDGE ( 'NONE', *, *, #6125, .F. ) ;
#17459 = ORIENTED_EDGE ( 'NONE', *, *, #3615, .F. ) ;
#17460 = VECTOR ( 'NONE', #2979, 1000.000000000000114 ) ;
#17461 = EDGE_LOOP ( 'NONE', ( #16540, #15730, #18337, #7811 ) ) ;
#17462 = ADVANCED_FACE ( 'NONE', ( #13033 ), #18105, .F. ) ;
#17463 = CARTESIAN_POINT ( 'NONE',  ( 16.72089543368710096, 0.4026526316987140142, 9.930969856814060748 ) ) ;
#17464 = LINE ( 'NONE', #10723, #6143 ) ;
#17465 = CYLINDRICAL_SURFACE ( 'NONE', #10386, 0.3962399999999975386 ) ;
#17466 = LINE ( 'NONE', #17358, #20624 ) ;
#17467 = CARTESIAN_POINT ( 'NONE',  ( 3.584452600926797849, 16.72241728061646526, 9.195045433009065405 ) ) ;
#17468 = VERTEX_POINT ( 'NONE', #8454 ) ;
#17469 = CARTESIAN_POINT ( 'NONE',  ( 5.716839746668139988, 15.72743057685165802, 8.084269252690832630 ) ) ;
#17470 = AXIS2_PLACEMENT_3D ( 'NONE', #39, #6791, #2019 ) ;
#17471 = FACE_OUTER_BOUND ( 'NONE', #18842, .T. ) ;
#17472 = DIRECTION ( 'NONE',  ( 0.9685006480810791629, -1.017240852913530016E-16, 0.2490110332224850231 ) ) ;
#17473 = FACE_OUTER_BOUND ( 'NONE', #3724, .T. ) ;
#17474 = DIRECTION ( 'NONE',  ( 0.000000000000000000, 1.000000000000000000, 0.000000000000000000 ) ) ;
#17475 = ORIENTED_EDGE ( 'NONE', *, *, #10458, .F. ) ;
#17476 = ORIENTED_EDGE ( 'NONE', *, *, #6005, .F. ) ;
#17477 = ADVANCED_FACE ( 'NONE', ( #6808 ), #13569, .F. ) ;
#17478 = CARTESIAN_POINT ( 'NONE',  ( 12.54513423051922949, 22.19922814609550343, 0.4896788010615997777 ) ) ;
#17479 = EDGE_CURVE ( 'NONE', #16565, #17254, #6491, .T. ) ;
#17481 = DIRECTION ( 'NONE',  ( 0.000000000000000000, 1.000000000000000000, 0.000000000000000000 ) ) ;
#17480 = LINE ( 'NONE', #13649, #20337 ) ;
#17482 = CARTESIAN_POINT ( 'NONE',  ( 12.41603076232164149, 10.50003331104365145, 2.481808480734982503 ) ) ;
#17483 = ORIENTED_EDGE ( 'NONE', *, *, #4121, .T. ) ;
#17484 = AXIS2_PLACEMENT_3D ( 'NONE', #9046, #14279, #9152 ) ;
#17485 = ORIENTED_EDGE ( 'NONE', *, *, #14460, .T. ) ;
#17486 = CARTESIAN_POINT ( 'NONE',  ( 13.36585934105912976, 21.37707621349031228, 1.842755075219712380 ) ) ;
#17487 = CARTESIAN_POINT ( 'NONE',  ( 7.739444420806847802, 11.44787533346460329, -0.07146953005562114991 ) ) ;
#17488 = LINE ( 'NONE', #2331, #9071 ) ;
#17489 = FACE_BOUND ( 'NONE', #20259, .T. ) ;
#17490 = CARTESIAN_POINT ( 'NONE',  ( 6.121636652558352765, 11.97495218357331126, 1.622048758636034371 ) ) ;
#17491 = CARTESIAN_POINT ( 'NONE',  ( 7.159321783504445591, 13.10796198399429180, 6.354849902668623152 ) ) ;
#17492 = DIRECTION ( 'NONE',  ( 0.000000000000000000, -1.000000000000000000, 0.000000000000000000 ) ) ;
#17493 = CARTESIAN_POINT ( 'NONE',  ( 9.357486251614197670, 15.29706862181782512, -3.643147517251545953 ) ) ;
#17494 = EDGE_CURVE ( 'NONE', #4294, #9387, #6018, .T. ) ;
#17495 = CIRCLE ( 'NONE', #3024, 0.3962399999999988154 ) ;
#17496 = DIRECTION ( 'NONE',  ( 0.000000000000000000, 0.000000000000000000, -1.000000000000000000 ) ) ;
#17497 = CARTESIAN_POINT ( 'NONE',  ( 1.654834657223931416, 13.92071940861192658, 9.115514740275299843 ) ) ;
#17498 = CARTESIAN_POINT ( 'NONE',  ( 1.199470371641251809, 19.13002063928019680, 8.749493374470841189 ) ) ;
#17499 = DIRECTION ( 'NONE',  ( -0.3482992169606098365, 0.9330960544336215357, -0.08955115110948595747 ) ) ;
#17500 = CARTESIAN_POINT ( 'NONE',  ( 3.684248113294236404, 15.57273015692113560, -0.6781872857148856237 ) ) ;
#17501 = DIRECTION ( 'NONE',  ( -0.3542738219355860418, 0.000000000000000000, -0.9351417320872557060 ) ) ;
#17502 = DIRECTION ( 'NONE',  ( 0.000000000000000000, 1.000000000000000000, 0.000000000000000000 ) ) ;
#17503 = CARTESIAN_POINT ( 'NONE',  ( 20.45273674534495711, -0.7129475169430978809, -14.09995496590185304 ) ) ;
#17504 = CYLINDRICAL_SURFACE ( 'NONE', #15244, 0.5080000000000000071 ) ;
#17505 = EDGE_CURVE ( 'NONE', #4458, #15970, #9891, .T. ) ;
#17506 = DIRECTION ( 'NONE',  ( 0.000000000000000000, 0.000000000000000000, -1.000000000000000000 ) ) ;
#17507 = CARTESIAN_POINT ( 'NONE',  ( 10.30969903151489753, 10.57682959022645086, 2.198775769149219794 ) ) ;
#17508 = ORIENTED_EDGE ( 'NONE', *, *, #12874, .T. ) ;
#17509 = FACE_OUTER_BOUND ( 'NONE', #1318, .T. ) ;
#17510 = CARTESIAN_POINT ( 'NONE',  ( 11.39871391131987544, 18.20778558999124996, -3.270776772179419201 ) ) ;
#17511 = CARTESIAN_POINT ( 'NONE',  ( 5.418943138485480482, 16.68965774897775844, -2.152926305030879561 ) ) ;
#17512 = CARTESIAN_POINT ( 'NONE',  ( 37.09580597189848561, 38.88803500000000213, 2.672127428255844261 ) ) ;
#17513 = ORIENTED_EDGE ( 'NONE', *, *, #1932, .F. ) ;
#17514 = AXIS2_PLACEMENT_3D ( 'NONE', #5116, #355, #17052 ) ;
#17515 = CARTESIAN_POINT ( 'NONE',  ( 71.03963378001139972, 1.984375000000000000, -10.54138470677948014 ) ) ;
#17516 = DIRECTION ( 'NONE',  ( 0.000000000000000000, 1.000000000000000000, 0.000000000000000000 ) ) ;
#17517 = CARTESIAN_POINT ( 'NONE',  ( 21.32189013745294659, -2.645762206214888224, -13.94514596636895298 ) ) ;
#17518 = VERTEX_POINT ( 'NONE', #10020 ) ;
#17519 = CARTESIAN_POINT ( 'NONE',  ( 11.29885047147741872, 14.04693538215814108, 6.356497555191443993 ) ) ;
#17520 = ADVANCED_FACE ( 'NONE', ( #4729 ), #13458, .T. ) ;
#17521 = CARTESIAN_POINT ( 'NONE',  ( 5.997264362299300267, 18.80374057110937969, -0.8573060022457920093 ) ) ;
#17522 = CARTESIAN_POINT ( 'NONE',  ( 2.162650458241309526, 21.20295136681662385, 4.895597986950482650 ) ) ;
#17523 = ADVANCED_FACE ( 'NONE', ( #3492 ), #9792, .F. ) ;
#17524 = CARTESIAN_POINT ( 'NONE',  ( 70.64340948846358970, 0.000000000000000000, -10.53785647675949910 ) ) ;
#17525 = ADVANCED_FACE ( 'NONE', ( #15343 ), #12397, .T. ) ;
#17526 = CARTESIAN_POINT ( 'NONE',  ( 48.78323016782857735, 34.52875999999999834, -25.79158832643865651 ) ) ;
#17527 = CARTESIAN_POINT ( 'NONE',  ( 19.75297330285050279, -2.349405567017404106, -14.22479102338560253 ) ) ;
#17528 = CYLINDRICAL_SURFACE ( 'NONE', #19428, 0.7950200000000000600 ) ;
#17529 = ORIENTED_EDGE ( 'NONE', *, *, #14301, .T. ) ;
#17530 =( REPRESENTATION_RELATIONSHIP ('NONE','NONE', #15554, #10883 ) REPRESENTATION_RELATIONSHIP_WITH_TRANSFORMATION ( #21358 )SHAPE_REPRESENTATION_RELATIONSHIP( ) );
#17531 = CARTESIAN_POINT ( 'NONE',  ( 7.869492175089545682, 20.10324751469710236, -1.674706184886148197 ) ) ;
#17532 = CARTESIAN_POINT ( 'NONE',  ( 12.13621795668766445, -3.968114999999999615, 4.225309685850866082 ) ) ;
#17533 = ORIENTED_EDGE ( 'NONE', *, *, #15793, .T. ) ;
#17534 = CARTESIAN_POINT ( 'NONE',  ( 10.33879874242046881, 11.37625080756972196, 2.332289602398126327 ) ) ;
#17535 = DIRECTION ( 'NONE',  ( 0.000000000000000000, 1.000000000000000000, 0.000000000000000000 ) ) ;
#17536 = DIRECTION ( 'NONE',  ( -0.3542738219355860418, 0.000000000000000000, -0.9351417320872557060 ) ) ;
#17538 = CARTESIAN_POINT ( 'NONE',  ( 14.05820270259704152, 128.5105379999999968, -15.03781736451272444 ) ) ;
#17537 = CARTESIAN_POINT ( 'NONE',  ( 6.821800543401555394, 11.73277151300288246, 6.051479129978276639 ) ) ;
#17539 = ORIENTED_EDGE ( 'NONE', *, *, #6248, .F. ) ;
#17540 = CARTESIAN_POINT ( 'NONE',  ( 7.539611788425835570, 15.71225078316309087, 8.356678781641505793 ) ) ;
#17541 = DIRECTION ( 'NONE',  ( 0.8609107660235850723, 0.000000000000000000, -0.5087559856598092844 ) ) ;
#17542 = CARTESIAN_POINT ( 'NONE',  ( 38.96848998618624904, -7.547609999999999708, -3.934807454472129429 ) ) ;
#17543 = ORIENTED_EDGE ( 'NONE', *, *, #1308, .F. ) ;
#17544 = CARTESIAN_POINT ( 'NONE',  ( 19.33880417540428098, 0.3883429578762613854, -15.04034309088197574 ) ) ;
#17545 = CARTESIAN_POINT ( 'NONE',  ( 0.07524201242303449333, 14.12641634776789701, 1.440853565142458548 ) ) ;
#17546 = CARTESIAN_POINT ( 'NONE',  ( 19.41828633390691294, -5.355847088986745774, -14.13626125933856592 ) ) ;
#17547 = EDGE_LOOP ( 'NONE', ( #485, #11061, #20777, #1287 ) ) ;
#17548 = CARTESIAN_POINT ( 'NONE',  ( 32.55306802826559220, 34.52875999999999834, -17.37731658638881527 ) ) ;
#17549 = CARTESIAN_POINT ( 'NONE',  ( 2.167054928856627427, 18.10873905883254054, 0.4144402421202247888 ) ) ;
#17550 = DIRECTION ( 'NONE',  ( -0.000000000000000000, -1.000000000000000000, 0.000000000000000000 ) ) ;
#17551 = EDGE_CURVE ( 'NONE', #9160, #16425, #21741, .T. ) ;
#17552 = AXIS2_PLACEMENT_3D ( 'NONE', #21763, #14726, #11492 ) ;
#17553 = DIRECTION ( 'NONE',  ( 0.000000000000000000, 1.000000000000000000, 0.000000000000000000 ) ) ;
#17554 = CYLINDRICAL_SURFACE ( 'NONE', #9782, 11.02160133116777452 ) ;
#17555 = ORIENTED_EDGE ( 'NONE', *, *, #5447, .F. ) ;
#17556 = LINE ( 'NONE', #5722, #12496 ) ;
#17558 = CARTESIAN_POINT ( 'NONE',  ( 13.39756118469465029, 22.16307784260286340, 1.948616576935187750 ) ) ;
#17557 = CARTESIAN_POINT ( 'NONE',  ( 54.36523883999320361, 1.984375000000000000, -30.28170612544299800 ) ) ;
#17559 = VERTEX_POINT ( 'NONE', #58 ) ;
#17560 = VERTEX_POINT ( 'NONE', #21630 ) ;
#17562 = LINE ( 'NONE', #19315, #382 ) ;
#17561 = CARTESIAN_POINT ( 'NONE',  ( 5.170513987664465461, 19.21498006567040306, 8.068247906139180969 ) ) ;
#17563 = ORIENTED_EDGE ( 'NONE', *, *, #21197, .T. ) ;
#17564 = CARTESIAN_POINT ( 'NONE',  ( 5.308873048291212093, 12.30939206186834234, 6.978150703179593073 ) ) ;
#17565 = VERTEX_POINT ( 'NONE', #20060 ) ;
#17566 = AXIS2_PLACEMENT_3D ( 'NONE', #3509, #7272, #3736 ) ;
#17567 = ORIENTED_EDGE ( 'NONE', *, *, #10354, .T. ) ;
#17568 = ORIENTED_EDGE ( 'NONE', *, *, #15268, .F. ) ;
#17569 = CARTESIAN_POINT ( 'NONE',  ( 2.833759500333274506, 12.12335935744747673, 5.064409189712415049 ) ) ;
#17570 = ADVANCED_FACE ( 'NONE', ( #18418 ), #19855, .T. ) ;
#17571 = DIRECTION ( 'NONE',  ( 0.9876802608827760510, 0.000000000000000000, -0.1564854698127960131 ) ) ;
#17572 = CARTESIAN_POINT ( 'NONE',  ( 29.36874999999999858, 22.62187499999999929, 10.71562499999999929 ) ) ;
#17573 = LINE ( 'NONE', #12709, #21698 ) ;
#17574 = CARTESIAN_POINT ( 'NONE',  ( 3.360528770871516357, 18.30797757280501514, 8.812766717346661949 ) ) ;
#17575 = ORIENTED_EDGE ( 'NONE', *, *, #21140, .T. ) ;
#17576 = CARTESIAN_POINT ( 'NONE',  ( 3.203589963913604510, 20.27761254839711924, 2.059023497881901310 ) ) ;
#17577 = DIRECTION ( 'NONE',  ( 0.000000000000000000, 1.000000000000000000, 0.000000000000000000 ) ) ;
#17578 = DIRECTION ( 'NONE',  ( 0.000000000000000000, 1.000000000000000000, 0.000000000000000000 ) ) ;
#17579 = CARTESIAN_POINT ( 'NONE',  ( 0.2641497867371597752, 3.961447500000001565, -24.43980549416641068 ) ) ;
#17580 = CARTESIAN_POINT ( 'NONE',  ( 36.51250000000000284, 32.54502000000000095, -10.31875000000000142 ) ) ;
#17581 = VERTEX_POINT ( 'NONE', #19963 ) ;
#17582 = ORIENTED_EDGE ( 'NONE', *, *, #3484, .F. ) ;
#17583 = EDGE_CURVE ( 'NONE', #6627, #2217, #4835, .T. ) ;
#17584 = CARTESIAN_POINT ( 'NONE',  ( 10.64102610220981404, 14.18796137044646777, -3.896004485940504303 ) ) ;
#17586 = CARTESIAN_POINT ( 'NONE',  ( -7.545238043312568088, -1.594802499999999013, -33.79351368943453338 ) ) ;
#17585 = DIRECTION ( 'NONE',  ( -0.4987171968201988270, 0.000000000000000000, 0.8667647648559574369 ) ) ;
#17587 = CARTESIAN_POINT ( 'NONE',  ( 12.77823618144881657, 11.02768345846162212, 4.001507650519105397 ) ) ;
#17588 = ORIENTED_EDGE ( 'NONE', *, *, #20797, .T. ) ;
#17589 = ORIENTED_EDGE ( 'NONE', *, *, #12995, .T. ) ;
#17590 = CARTESIAN_POINT ( 'NONE',  ( 44.27024749654656688, -9.531985000000000596, -8.722764363618033201 ) ) ;
#17591 = CARTESIAN_POINT ( 'NONE',  ( 7.880086733409702227, 20.03079912825525355, -1.576550733578341301 ) ) ;
#17592 = CARTESIAN_POINT ( 'NONE',  ( -29.36874999999999858, 30.56128000000000000, 10.71562499999999929 ) ) ;
#17593 = DIRECTION ( 'NONE',  ( 0.1060008583745224581, 0.000000000000000000, 0.9943660382494288186 ) ) ;
#17594 = CARTESIAN_POINT ( 'NONE',  ( 8.260560628456950383, 20.28274240130079065, 5.104618557005875523 ) ) ;
#17595 = CIRCLE ( 'NONE', #16542, 2.579687500000000355 ) ;
#17596 = FACE_OUTER_BOUND ( 'NONE', #1970, .T. ) ;
#17597 = EDGE_CURVE ( 'NONE', #723, #18266, #3165, .T. ) ;
#17598 = EDGE_CURVE ( 'NONE', #15912, #18286, #15176, .T. ) ;
#17599 = PRODUCT_DEFINITION_FORMATION_WITH_SPECIFIED_SOURCE ( 'ANY', '', #4744, .NOT_KNOWN. ) ;
#17600 = CARTESIAN_POINT ( 'NONE',  ( 1.869412468721153076, 18.25238594264126135, -0.4582093693669330725 ) ) ;
#17601 = CARTESIAN_POINT ( 'NONE',  ( 0.7473452975581560409, 20.25628870484626631, 7.621704803408686502 ) ) ;
#17602 = DIRECTION ( 'NONE',  ( 0.2490110332224850509, 0.000000000000000000, -0.9685006480810792739 ) ) ;
#17603 = CARTESIAN_POINT ( 'NONE',  ( -0.8210072273473643101, 19.84627995571224091, 3.577383950576946692 ) ) ;
#17604 = DIRECTION ( 'NONE',  ( 0.2868778675745004558, 0.000000000000000000, 0.9579671649362035968 ) ) ;
#17605 = CARTESIAN_POINT ( 'NONE',  ( 46.03750000000000142, 0.000000000000000000, -10.31874999999999964 ) ) ;
#17606 = CARTESIAN_POINT ( 'NONE',  ( 20.56352968641046886, -0.9909231540084149081, -14.06044304150320556 ) ) ;
#17607 = ORIENTED_EDGE ( 'NONE', *, *, #18429, .T. ) ;
#17608 = CARTESIAN_POINT ( 'NONE',  ( 49.09065990372640442, 32.54502000000000095, -26.70549589918839928 ) ) ;
#17609 = VECTOR ( 'NONE', #8548, 1000.000000000000000 ) ;
#17610 = CARTESIAN_POINT ( 'NONE',  ( 11.21047793104343704, 12.39978222132418573, 6.074997740956973757 ) ) ;
#17611 = ORIENTED_EDGE ( 'NONE', *, *, #2078, .T. ) ;
#17612 = B_SPLINE_SURFACE_WITH_KNOTS ( 'NONE', 3, 3, ( 
 ( #18553, #10048, #13380, #4957, #11711, #1211, #15264, #5390, #8807, #20751, #7050, #5607, #10377, #11923, #15377, #3635, #20302, #17339, #8485, #12154, #5171, #5496, #13939, #15705, #5272, #1964, #16896, #1745, #15584, #91, #12033, #8702, #2066, #15481, #12367, #17224, #533, #307, #18878, #18653, #2187, #423, #20636, #7174, #18981, #13601, #18766, #14043, #12258, #17124, #3854, #3963, #3749, #19093, #10592, #6842, #200, #6942, #8928, #7282, #13706, #3521, #10257, #17005, #20405, #1858, #13818 ),
 ( #20523, #10482, #8601, #634, #16130, #5729, #19418, #7603, #2411, #20979, #4406, #12484, #14262, #14364, #17668, #9137, #959, #6162, #16240, #1070, #19636, #19206, #2297, #21080, #21299, #12927, #11032, #4073, #21186, #5832, #861, #5930, #10814, #10708, #2634, #7813, #14591, #17453, #9033, #6044, #17561, #7496, #11140, #15922, #12590, #17888, #2521, #15808, #7384, #14154, #20858, #19314, #14469, #744, #4176, #10919, #9251, #12815, #4292, #16030, #12694, #17787, #9363, #7709, #19541, #2734, #9470 ),
 ( #19964, #13256, #18419, #6595, #10021, #21742, #4836, #6371, #1393, #21632, #2845, #14916, #18311, #8356, #16561, #15126, #19857, #21407, #2964, #13143, #7927, #4931, #17989, #6492, #14703, #15025, #1507, #3290, #14806, #11470, #4504, #11241, #3167, #9577, #21514, #18215, #11571, #3067, #21845, #9898, #16774, #9793, #16664, #6262, #11679, #8252, #13356, #20061, #1615, #1185, #4730, #6699, #13460, #8135, #16347, #13034, #19738, #4612, #11357, #18107, #9690, #16456, #1292, #8030, #1936, #5246, #18627 ),
 ( #3827, #7260, #6812, #11795, #8678, #8900, #15680, #20493, #15229, #8781, #8571, #10347, #17091, #13571, #20171, #12126, #10562, #17308, #5046, #2155, #15561, #60, #16975, #13914, #20275, #174, #5469, #12006, #509, #18528, #3393, #10127, #6916, #2036, #5146, #15346, #11898, #3494, #393, #7021, #16872, #10230, #18737, #15452, #1719, #7147, #1829, #20611, #8457, #13679, #20379, #279, #3607, #13789, #18955, #5364, #18850, #3718, #10459, #12231, #17196, #613, #17537, #9446, #721, #7581, #1045 ),
 ( #7469, #17431, #14446, #5579, #9227, #2272, #2607, #11002, #12790, #2385, #20957, #14019, #20723, #12671, #12338, #9112, #5813, #21058, #12569, #16218, #14343, #19513, #19292, #16007, #9011, #21163, #19393, #17761, #5909, #939, #10684, #15895, #11115, #4264, #14240, #9337, #19064, #2493, #3938, #7686, #17867, #12459, #4048, #6019, #4381, #19182, #2712, #15786, #7358, #14128, #20831, #5699, #10792, #4154, #10892, #836, #17641, #9869, #13333, #3145, #1365, #14779, #4706, #3044, #6133, #14885, #21604 ),
 ( #14558, #6466, #3260, #4904, #11331, #9996, #6344, #11446, #21277, #13230, #19940, #17970, #4813, #2820, #21718, #9556, #11546, #18284, #11981, #8654, #1592, #13431, #17173, #12099, #13765, #15323, #8427, #6783, #18710, #18823, #20465, #1799, #5017, #20250, #3690, #3579, #11875, #6892, #2013, #10318, #10434, #18497, #20354, #18603, #10204, #3369, #20142, #6994, #10101, #17063, #5223, #15203, #3470, #8754, #16848, #5125, #1909, #8542, #31, #15535, #18931, #7116, #13885, #10536, #1688, #15103, #15428 ),
 ( #16948, #145, #365, #20583, #5443, #3801, #11772, #13544, #8334, #21817, #3913, #20696, #918, #19484, #5673, #10655, #15763, #2358, #5554, #2582, #12432, #19159, #4026, #7440, #10770, #14215, #15866, #19272, #20929, #5789, #12548, #15982, #813, #14321, #5886, #6437, #6105, #7873, #4786, #4462, #12984, #18259, #18052, #6549, #2693, #20012, #16195, #19693, #14860, #11194, #21356, #19596, #12877, #13203, #19802, #1020, #17946, #2910, #14756, #13310, #19915, #2794, #21575, #14534, #9530, #21691, #7985 ),
 ( #6213, #9640, #8202, #16406, #11516, #11094, #16298, #14650, #17847, #4562, #4678, #9422, #11420, #14976, #1454, #1133, #7767, #1242, #21462, #21253, #11305, #6319, #13092, #18168, #3019, #3120, #9744, #16507, #1343, #8085, #9844, #16614, #13522, #17259, #5419, #13856, #15409, #8517, #6872, #12070, #18908, #20558, #1886, #5102, #20329, #12184, #18797, #11953, #6971, #2100, #10412, #10513, #18581, #20435, #18684, #10290, #3444, #20229, #7086, #10179, #17154, #5305, #15298, #3552, #8846, #16923, #5203 ),
 ( #15625, #3666, #3779, #463, #7211, #1770, #17040, #1994, #20670, #13973, #5530, #8633, #231, #13741, #12289, #8735, #19014, #6756, #122, #15511, #341, #13631, #11850, #3889, #10627, #1664, #8402, #15178, #7, #12520, #2445, #11066, #9287, #19131, #17703, #14075, #4000, #19452, #9170, #567, #21111, #14398, #7414, #19243, #12728, #4105, #2555, #4327, #12405, #669, #17821, #20896, #14295, #17380, #21015, #2222, #8962, #14188, #15739, #15953, #7532, #20782, #5763, #5861, #5644, #9065, #7311 ) ),
 .UNSPECIFIED., .F., .F., .F.,
 ( 4, 1, 1, 1, 1, 1, 4 ),
 ( 4, 1, 1, 1, 1, 1, 1, 1, 1, 1, 1, 1, 1, 1, 1, 1, 1, 1, 1, 1, 1, 1, 1, 1, 1, 1, 1, 1, 1, 1, 1, 1, 1, 1, 1, 1, 1, 1, 1, 1, 1, 1, 1, 1, 1, 1, 1, 1, 1, 1, 1, 1, 1, 1, 1, 1, 1, 1, 1, 1, 1, 1, 1, 1, 4 ),
 ( 0.4887878733748999838, 0.5000000000000000000, 0.6250000000000000000, 0.7500000000000000000, 0.8750000000000000000, 1.000000000000000000, 1.011212126625000041 ),
 ( -0.02000000000000000042, -0.003749999999999999861, 0.01250000000000000069, 0.02875000000000000125, 0.04499999999999999833, 0.06124999999999999889, 0.07749999999999999944, 0.09375000000000000000, 0.1100000000000000006, 0.1262500000000000011, 0.1424999999999999878, 0.1587500000000000022, 0.1749999999999999889, 0.1912500000000000033, 0.2074999999999999900, 0.2237500000000000044, 0.2399999999999999911, 0.2562499999999999778, 0.2725000000000000200, 0.2887500000000000067, 0.3049999999999999933, 0.3212499999999999800, 0.3375000000000000222, 0.3537500000000000089, 0.3699999999999999956, 0.3862499999999999822, 0.4025000000000000244, 0.4187500000000000111, 0.4349999999999999978, 0.4512499999999999845, 0.4675000000000000266, 0.4837500000000000133, 0.5000000000000000000, 0.5162499999999999867, 0.5324999999999999734, 0.5487499999999999600, 0.5649999999999999467, 0.5812500000000000444, 0.5975000000000000311, 0.6137500000000000178, 0.6300000000000000044, 0.6462499999999999911, 0.6624999999999999778, 0.6787499999999999645, 0.6949999999999999512, 0.7112500000000000488, 0.7275000000000000355, 0.7437500000000000222, 0.7600000000000000089, 0.7762499999999999956, 0.7924999999999999822, 0.8087499999999999689, 0.8249999999999999556, 0.8412500000000000533, 0.8575000000000000400, 0.8737500000000000266, 0.8900000000000000133, 0.9062500000000000000, 0.9224999999999999867, 0.9387499999999999734, 0.9549999999999999600, 0.9712499999999999467, 0.9875000000000000444, 1.003749999999999920, 1.020000000000000018 ),
 .UNSPECIFIED. ) ;
#17613 = CARTESIAN_POINT ( 'NONE',  ( 49.41195815393805901, 42.06303499999999929, -1.411525001868561224 ) ) ;
#17614 = CARTESIAN_POINT ( 'NONE',  ( 6.107171055585940422, 11.13133987716735973, 1.634779367331249844 ) ) ;
#17615 = DIRECTION ( 'NONE',  ( -0.9685006480810791629, 0.000000000000000000, -0.2490110332224850231 ) ) ;
#17616 = ORIENTED_EDGE ( 'NONE', *, *, #9786, .F. ) ;
#17617 = EDGE_CURVE ( 'NONE', #11228, #8566, #8437, .T. ) ;
#17618 = VECTOR ( 'NONE', #8984, 1000.000000000000114 ) ;
#17619 = CARTESIAN_POINT ( 'NONE',  ( -0.1849527131266449076, 20.23672349358593792, 5.150944217628095068 ) ) ;
#17620 = CARTESIAN_POINT ( 'NONE',  ( 5.674198503080612355, 20.72820056094829866, 3.861845262972528836 ) ) ;
#17621 = CARTESIAN_POINT ( 'NONE',  ( 9.828862065001116477, -3.968114999999999615, -16.12522240043857025 ) ) ;
#17622 = EDGE_CURVE ( 'NONE', #21599, #7945, #15570, .T. ) ;
#17623 = VECTOR ( 'NONE', #9358, 1000.000000000000114 ) ;
#17624 = ORIENTED_EDGE ( 'NONE', *, *, #21261, .T. ) ;
#17625 = CARTESIAN_POINT ( 'NONE',  ( 13.90474715608841905, 20.92783617524978013, 3.353010216828454126 ) ) ;
#17626 = EDGE_CURVE ( 'NONE', #5142, #13568, #2640, .T. ) ;
#17627 = CARTESIAN_POINT ( 'NONE',  ( 12.03200418959231932, 11.13144644120788307, 0.7512433199295541764 ) ) ;
#17628 = CARTESIAN_POINT ( 'NONE',  ( 1.992131233281914993, 16.44430802189885199, -0.8027766641775135881 ) ) ;
#17629 = FACE_OUTER_BOUND ( 'NONE', #20350, .T. ) ;
#17630 = CARTESIAN_POINT ( 'NONE',  ( 4.183994795703180891, 21.11486309459522204, 5.551682479814725291 ) ) ;
#17631 = UNCERTAINTY_MEASURE_WITH_UNIT (LENGTH_MEASURE( 1.000000000000000082E-05 ), #6573, 'distance_accuracy_value', 'NONE');
#17632 = CARTESIAN_POINT ( 'NONE',  ( 53.10651001381376091, -5.166360000000002728, -16.70269254552787075 ) ) ;
#17633 = ORIENTED_EDGE ( 'NONE', *, *, #12053, .F. ) ;
#17634 = CARTESIAN_POINT ( 'NONE',  ( 9.323981051820602772, 11.74348662527086162, -1.552944996175415815 ) ) ;
#17635 = DIRECTION ( 'NONE',  ( 0.000000000000000000, 1.000000000000000000, 0.000000000000000000 ) ) ;
#17636 = VERTEX_POINT ( 'NONE', #20721 ) ;
#17637 = CARTESIAN_POINT ( 'NONE',  ( 9.914072323211984283, 11.61724307103066245, 0.4831293664772999819 ) ) ;
#17638 = AXIS2_PLACEMENT_3D ( 'NONE', #14234, #7576, #9219 ) ;
#17639 = DIRECTION ( 'NONE',  ( -0.9685006480810792739, 0.000000000000000000, -0.2490110332224846346 ) ) ;
#17640 = CARTESIAN_POINT ( 'NONE',  ( 1.327966776992419939, 17.25716549828085888, 8.748930041179065142 ) ) ;
#17642 = DIRECTION ( 'NONE',  ( -0.3482992169606098365, 0.9330960544336215357, -0.08955115110948595747 ) ) ;
#17641 = CARTESIAN_POINT ( 'NONE',  ( 5.815434679165389475, 20.81351436963172219, 5.507186064765134503 ) ) ;
#17643 = EDGE_LOOP ( 'NONE', ( #13222, #21628, #18987, #12477, #6525, #1420, #17567, #5701, #18447, #4605, #21812, #21447, #3051, #15341, #18296, #15147, #15591, #15313, #1831, #10274, #5952, #6806, #9636, #19735, #4207, #20967, #7184 ) ) ;
#17644 = DIRECTION ( 'NONE',  ( 1.000000000000000000, 0.000000000000000000, 0.000000000000000000 ) ) ;
#17645 = ADVANCED_FACE ( 'NONE', ( #15559 ), #2153, .F. ) ;
#17646 = DIRECTION ( 'NONE',  ( -0.08420877549337300871, 0.000000000000000000, -0.9964481331860212121 ) ) ;
#17647 = EDGE_CURVE ( 'NONE', #5639, #12509, #11277, .T. ) ;
#17648 = CARTESIAN_POINT ( 'NONE',  ( -3.042350287543033716, 2.373947500000000765, -26.17378113315171007 ) ) ;
#17649 = VECTOR ( 'NONE', #1478, 1000.000000000000000 ) ;
#17650 = EDGE_CURVE ( 'NONE', #19545, #12822, #2383, .T. ) ;
#17651 = VERTEX_POINT ( 'NONE', #4046 ) ;
#17652 = CARTESIAN_POINT ( 'NONE',  ( 19.36991330292439173, 0.2418614478177981975, -15.04532736253224989 ) ) ;
#17653 = CARTESIAN_POINT ( 'NONE',  ( 14.82073529532191714, -7.423173529680283877, -15.07752894836403890 ) ) ;
#17654 = EDGE_LOOP ( 'NONE', ( #10884, #18306, #15027, #20822 ) ) ;
#17655 = DIRECTION ( 'NONE',  ( 0.000000000000000000, 1.000000000000000000, 0.000000000000000000 ) ) ;
#17656 = CARTESIAN_POINT ( 'NONE',  ( 1.891993562269222329, 15.79923009215404583, 0.1066366400433323702 ) ) ;
#17657 = CARTESIAN_POINT ( 'NONE',  ( 11.82678039945931481, -3.968114999999999615, -12.74436900065013667 ) ) ;
#17658 = CARTESIAN_POINT ( 'NONE',  ( -23.81250000000000000, 16.27314499999999953, 10.71562499999999929 ) ) ;
#17659 = DIRECTION ( 'NONE',  ( 0.000000000000000000, -1.000000000000000000, -0.000000000000000000 ) ) ;
#17660 = ORIENTED_EDGE ( 'NONE', *, *, #14790, .F. ) ;
#17661 = DIRECTION ( 'NONE',  ( 0.000000000000000000, 1.000000000000000000, 0.000000000000000000 ) ) ;
#17662 = VECTOR ( 'NONE', #10116, 1000.000000000000000 ) ;
#17664 = DIRECTION ( 'NONE',  ( 0.000000000000000000, 1.000000000000000000, 0.000000000000000000 ) ) ;
#17663 = LINE ( 'NONE', #2512, #9145 ) ;
#17665 = ORIENTED_EDGE ( 'NONE', *, *, #13537, .T. ) ;
#17666 = ORIENTED_EDGE ( 'NONE', *, *, #12659, .T. ) ;
#17667 = CARTESIAN_POINT ( 'NONE',  ( 46.03750000000000142, 42.06303499999999929, -10.31874999999999964 ) ) ;
#17668 = CARTESIAN_POINT ( 'NONE',  ( -0.1496539994742919766, 13.90840449083211183, 0.5606114275089872923 ) ) ;
#17669 = ORIENTED_EDGE ( 'NONE', *, *, #13561, .F. ) ;
#17670 = CARTESIAN_POINT ( 'NONE',  ( 3.679434963568711581, 17.70425422745077526, -1.266375082759285231 ) ) ;
#17671 = EDGE_CURVE ( 'NONE', #6512, #12008, #2134, .T. ) ;
#17672 = ORIENTED_EDGE ( 'NONE', *, *, #15360, .F. ) ;
#17673 = EDGE_CURVE ( 'NONE', #20432, #4259, #18036, .T. ) ;
#17674 = VECTOR ( 'NONE', #11956, 1000.000000000000000 ) ;
#17675 = EDGE_LOOP ( 'NONE', ( #4935, #6665, #2157, #11848 ) ) ;
#17676 = CARTESIAN_POINT ( 'NONE',  ( 1.223645171401676501, 12.88107361349177715, 7.032740771049156514 ) ) ;
#17677 = ORIENTED_EDGE ( 'NONE', *, *, #14508, .T. ) ;
#17678 = VECTOR ( 'NONE', #7428, 1000.000000000000000 ) ;
#17679 = CARTESIAN_POINT ( 'NONE',  ( 3.319333245867002624, 13.53315903595815151, 7.428627571892030268 ) ) ;
#17680 = DIRECTION ( 'NONE',  ( 0.000000000000000000, 1.000000000000000000, 0.000000000000000000 ) ) ;
#17681 = DIRECTION ( 'NONE',  ( -0.9685006480810792739, 0.000000000000000000, -0.2490110332224846346 ) ) ;
#17682 = CARTESIAN_POINT ( 'NONE',  ( 1.880866719892425376, 23.68649982446676816, 8.731249999999999289 ) ) ;
#17683 = CARTESIAN_POINT ( 'NONE',  ( 2.457276989675134526, 11.33093577474142144, 3.398861036160339744 ) ) ;
#17684 = AXIS2_PLACEMENT_3D ( 'NONE', #18769, #313, #10895 ) ;
#17685 = ORIENTED_EDGE ( 'NONE', *, *, #5107, .T. ) ;
#17686 = AXIS2_PLACEMENT_3D ( 'NONE', #19858, #6596, #13357 ) ;
#17687 = CARTESIAN_POINT ( 'NONE',  ( 2.376677803493876251, 17.97529088148273502, 0.08679864734725686870 ) ) ;
#17688 = LINE ( 'NONE', #2539, #15275 ) ;
#17689 = LINE ( 'NONE', #17807, #17739 ) ;
#17690 = CARTESIAN_POINT ( 'NONE',  ( 56.47666780297049627, 36.51313500000000545, 1.109116340531466127 ) ) ;
#17691 = DIRECTION ( 'NONE',  ( 0.000000000000000000, 1.000000000000000000, 0.000000000000000000 ) ) ;
#17692 = ORIENTED_EDGE ( 'NONE', *, *, #21352, .T. ) ;
#17693 = VERTEX_POINT ( 'NONE', #611 ) ;
#17694 = CARTESIAN_POINT ( 'NONE',  ( 10.63866352414856031, 16.27132894921270534, -4.298429365974365091 ) ) ;
#17696 = CARTESIAN_POINT ( 'NONE',  ( 2.492193568723835462, 34.12394749999999988, -24.56873394466936134 ) ) ;
#17695 = CARTESIAN_POINT ( 'NONE',  ( -2.028188046367890074, 23.41816500000000190, 0.3682158094503220069 ) ) ;
#17697 = CARTESIAN_POINT ( 'NONE',  ( 11.42459273946487741, 11.33173356210819982, -1.660656841338600698 ) ) ;
#17698 = ORIENTED_EDGE ( 'NONE', *, *, #3696, .T. ) ;
#17699 = VERTEX_POINT ( 'NONE', #14124 ) ;
#17700 = ADVANCED_FACE ( 'NONE', ( #19061 ), #5362, .F. ) ;
#17701 = CARTESIAN_POINT ( 'NONE',  ( 2.651964239740473683, 13.08893749999999834, 5.873042593501262232 ) ) ;
#17702 = CARTESIAN_POINT ( 'NONE',  ( 7.444839536017474835, 18.18305382322718700, -2.602598617944788195 ) ) ;
#17703 = CARTESIAN_POINT ( 'NONE',  ( 2.128425141234220774, 17.94205954657215685, 0.2447211690924122052 ) ) ;
#17704 = DIRECTION ( 'NONE',  ( 0.000000000000000000, -1.000000000000000000, 0.000000000000000000 ) ) ;
#17705 = CARTESIAN_POINT ( 'NONE',  ( 7.477064758050143034, 20.91351444903647305, 3.036128329970051887 ) ) ;
#17706 = AXIS2_PLACEMENT_3D ( 'NONE', #18288, #8659, #6998 ) ;
#17707 = CIRCLE ( 'NONE', #17354, 1.190624999999997824 ) ;
#17708 = AXIS2_PLACEMENT_3D ( 'NONE', #21385, #21719, #15002 ) ;
#17709 = CARTESIAN_POINT ( 'NONE',  ( 67.79270099634359781, 1.984375000000000000, -13.76558698117381851 ) ) ;
#17710 = LINE ( 'NONE', #7218, #2104 ) ;
#17711 = CARTESIAN_POINT ( 'NONE',  ( 9.874098502813611233, 21.84389315528099829, 3.571521444139809098 ) ) ;
#17712 = DIRECTION ( 'NONE',  ( -0.000000000000000000, -1.000000000000000000, 0.000000000000000000 ) ) ;
#17713 = DIRECTION ( 'NONE',  ( -0.000000000000000000, -1.000000000000000000, 0.000000000000000000 ) ) ;
#17714 = CARTESIAN_POINT ( 'NONE',  ( -0.7439932220394867013, 20.80806006231328098, 3.735380117767566510 ) ) ;
#17715 = CARTESIAN_POINT ( 'NONE',  ( 1.227962039276562889, 11.89880261940416695, 6.900897714592743704 ) ) ;
#17716 = FACE_OUTER_BOUND ( 'NONE', #18099, .T. ) ;
#17717 = CARTESIAN_POINT ( 'NONE',  ( 3.996171515784880057, 20.53258833712626341, 5.065504506774320959 ) ) ;
#17718 = DIRECTION ( 'NONE',  ( 0.000000000000000000, 1.000000000000000000, 0.000000000000000000 ) ) ;
#17719 = FACE_OUTER_BOUND ( 'NONE', #1256, .T. ) ;
#17720 = CARTESIAN_POINT ( 'NONE',  ( 11.45318987056821136, -0.2908542355871540641, -16.83281496953432210 ) ) ;
#17721 = CIRCLE ( 'NONE', #17374, 0.7950199999999985057 ) ;
#17722 = ORIENTED_EDGE ( 'NONE', *, *, #13591, .F. ) ;
#17723 = DIRECTION ( 'NONE',  ( 0.05085730733808139364, 0.000000000000000000, -0.9987059298363658577 ) ) ;
#17724 = AXIS2_PLACEMENT_3D ( 'NONE', #10756, #2349, #2459 ) ;
#17725 = VECTOR ( 'NONE', #20775, 1000.000000000000114 ) ;
#17726 = CARTESIAN_POINT ( 'NONE',  ( 11.30218536120831807, 12.95440410905304773, 6.520132354090415028 ) ) ;
#17727 = ORIENTED_EDGE ( 'NONE', *, *, #21824, .T. ) ;
#17728 = CARTESIAN_POINT ( 'NONE',  ( 24.28501924911759957, 0.9100045512280500182, 10.40023748037497953 ) ) ;
#17729 = EDGE_CURVE ( 'NONE', #4043, #19124, #13403, .T. ) ;
#17730 = AXIS2_PLACEMENT_3D ( 'NONE', #20219, #18248, #11940 ) ;
#17731 = CARTESIAN_POINT ( 'NONE',  ( 11.76196212326084378, 19.67897817189895449, -2.430607981699549835 ) ) ;
#17732 = CARTESIAN_POINT ( 'NONE',  ( 5.460238740336566643, 13.43797717707083805, -1.319921016749001863 ) ) ;
#17733 = LINE ( 'NONE', #16087, #14474 ) ;
#17734 = ORIENTED_EDGE ( 'NONE', *, *, #17897, .F. ) ;
#17735 =( NAMED_UNIT ( * ) PLANE_ANGLE_UNIT ( ) SI_UNIT ( $, .RADIAN. ) );
#17736 = CARTESIAN_POINT ( 'NONE',  ( 5.163813313501020019, 20.63322025226451473, 2.513191214141544005 ) ) ;
#17737 = CARTESIAN_POINT ( 'NONE',  ( 42.94469661997857912, 34.52875999999999834, -18.48251861828712705 ) ) ;
#17738 = AXIS2_PLACEMENT_3D ( 'NONE', #7719, #9480, #1080 ) ;
#17739 = VECTOR ( 'NONE', #5847, 1000.000000000000000 ) ;
#17740 = ORIENTED_EDGE ( 'NONE', *, *, #12211, .F. ) ;
#17741 = CARTESIAN_POINT ( 'NONE',  ( 11.81737553005730490, 19.71324643990528358, -2.564459159478865935 ) ) ;
#17742 = CARTESIAN_POINT ( 'NONE',  ( 13.16173767730900401, 16.70056792996117068, 6.496424000728083570 ) ) ;
#17743 = DIRECTION ( 'NONE',  ( 0.000000000000000000, -1.000000000000000000, 0.000000000000000000 ) ) ;
#17744 = AXIS2_PLACEMENT_3D ( 'NONE', #6065, #12836, #8476 ) ;
#17745 = COLOUR_RGB ( '', 0.66274510, 0.83137255, 0.94901961) ;
#17746 = CARTESIAN_POINT ( 'NONE',  ( 39.58386072796507449, 37.69740999999999786, -4.490541772578644064 ) ) ;
#17747 = DIRECTION ( 'NONE',  ( 0.000000000000000000, 1.000000000000000000, 0.000000000000000000 ) ) ;
#17748 = EDGE_CURVE ( 'NONE', #8949, #6430, #10212, .T. ) ;
#17749 = CARTESIAN_POINT ( 'NONE',  ( 3.495813267034087790, 21.35899666354531945, 3.686983560158256346 ) ) ;
#17750 = DIRECTION ( 'NONE',  ( 0.000000000000000000, 1.000000000000000000, 0.000000000000000000 ) ) ;
#17751 = ORIENTED_EDGE ( 'NONE', *, *, #21548, .F. ) ;
#17752 = CYLINDRICAL_SURFACE ( 'NONE', #17638, 1.785937499999999512 ) ;
#17753 = CIRCLE ( 'NONE', #19142, 0.7950200000000005041 ) ;
#17754 = VERTEX_POINT ( 'NONE', #20828 ) ;
#17755 = ADVANCED_FACE ( 'NONE', ( #10790 ), #15893, .F. ) ;
#17756 = CARTESIAN_POINT ( 'NONE',  ( 10.13769997516062560, 20.17993208692285023, -1.137326984910994376 ) ) ;
#17757 = CARTESIAN_POINT ( 'NONE',  ( -21.43124999999999858, 1.984375000000000000, -4.860316984116058095E-16 ) ) ;
#17758 = CARTESIAN_POINT ( 'NONE',  ( 1.289267033706648746, 17.50162684153391268, 8.689449867824082574 ) ) ;
#17759 = ADVANCED_FACE ( 'NONE', ( #8898 ), #5697, .F. ) ;
#17760 = EDGE_CURVE ( 'NONE', #1714, #11015, #391, .T. ) ;
#17762 = FACE_OUTER_BOUND ( 'NONE', #15575, .T. ) ;
#17761 = CARTESIAN_POINT ( 'NONE',  ( 2.779637312247832615, 12.24591714145684129, 6.811322434960999317 ) ) ;
#17763 = VERTEX_POINT ( 'NONE', #7019 ) ;
#17764 = CARTESIAN_POINT ( 'NONE',  ( -17.46249999999999858, 32.54247999999999763, 0.000000000000000000 ) ) ;
#17765 = AXIS2_PLACEMENT_3D ( 'NONE', #17090, #12230, #2271 ) ;
#17766 = CARTESIAN_POINT ( 'NONE',  ( 39.64083910660897203, -7.089776582593554366, -3.260385504968207115 ) ) ;
#17767 = ORIENTED_EDGE ( 'NONE', *, *, #2336, .T. ) ;
#17768 = AXIS2_PLACEMENT_3D ( 'NONE', #18965, #14029, #17320 ) ;
#17769 = CARTESIAN_POINT ( 'NONE',  ( -29.36874999999999858, 0.000000000000000000, -3.968750000000000000 ) ) ;
#17770 = CARTESIAN_POINT ( 'NONE',  ( 14.64275916103558650, -7.397369947662747691, -16.84371501784351466 ) ) ;
#17771 = EDGE_LOOP ( 'NONE', ( #19707, #11950, #4371, #15425 ) ) ;
#17772 = CARTESIAN_POINT ( 'NONE',  ( 47.80475250345343596, 38.88803500000000213, -11.91473563638196786 ) ) ;
#17773 = CIRCLE ( 'NONE', #94, 19.05000000000001137 ) ;
#17774 = CARTESIAN_POINT ( 'NONE',  ( 10.70530029303066044, 21.89451842192714182, 0.03457279810376413798 ) ) ;
#17775 = EDGE_CURVE ( 'NONE', #5934, #8566, #20377, .T. ) ;
#17776 = DIRECTION ( 'NONE',  ( -0.6050250551579474667, -0.7753173868113220069, 0.1811839737371539472 ) ) ;
#17777 = AXIS2_PLACEMENT_3D ( 'NONE', #16621, #1348, #6117 ) ;
#17778 = VERTEX_POINT ( 'NONE', #20491 ) ;
#17779 = CARTESIAN_POINT ( 'NONE',  ( 42.79471501377724252, -1.983739999999999837, 5.049205022181460834 ) ) ;
#17781 = CARTESIAN_POINT ( 'NONE',  ( 29.64606458365116737, 1.975802500000001904, -15.53894806404596096 ) ) ;
#17780 = CARTESIAN_POINT ( 'NONE',  ( 38.28489021960990613, 38.88803500000000213, 2.732679409805250703 ) ) ;
#17782 = EDGE_LOOP ( 'NONE', ( #11062, #5831, #2542, #14209 ) ) ;
#17783 = ORIENTED_EDGE ( 'NONE', *, *, #15047, .F. ) ;
#17784 = EDGE_CURVE ( 'NONE', #9498, #19225, #10344, .T. ) ;
#17785 = CARTESIAN_POINT ( 'NONE',  ( -13.87747867115857936, 36.51313500000000545, -9.458632424640695646 ) ) ;
#17786 = EDGE_CURVE ( 'NONE', #2943, #21869, #8779, .T. ) ;
#17788 = DIRECTION ( 'NONE',  ( 0.2490110332224857170, 0.000000000000000000, -0.9685006480810790519 ) ) ;
#17787 = CARTESIAN_POINT ( 'NONE',  ( 7.450947465380786561, 12.98226186039768137, 7.398020146545584375 ) ) ;
#17789 = ORIENTED_EDGE ( 'NONE', *, *, #1271, .T. ) ;
#17790 = CARTESIAN_POINT ( 'NONE',  ( 3.615277320435647646, 17.17694927600387800, -1.367159509867317713 ) ) ;
#17791 = AXIS2_PLACEMENT_3D ( 'NONE', #4283, #4399, #11134 ) ;
#17792 = VERTEX_POINT ( 'NONE', #13911 ) ;
#17793 = ORIENTED_EDGE ( 'NONE', *, *, #11625, .T. ) ;
#17794 = ORIENTED_EDGE ( 'NONE', *, *, #11808, .T. ) ;
#17795 = DIRECTION ( 'NONE',  ( 0.000000000000000000, 1.000000000000000000, 0.000000000000000000 ) ) ;
#17796 = EDGE_CURVE ( 'NONE', #20325, #9339, #3203, .T. ) ;
#17797 = CIRCLE ( 'NONE', #19550, 0.7950200000000003930 ) ;
#17798 = CARTESIAN_POINT ( 'NONE',  ( 9.256853431388732290, 36.51313500000000545, -17.09316853730597074 ) ) ;
#17799 = DIRECTION ( 'NONE',  ( 1.000000000000000000, 0.000000000000000000, 0.000000000000000000 ) ) ;
#17800 = DIRECTION ( 'NONE',  ( 0.000000000000000000, 1.000000000000000000, 0.000000000000000000 ) ) ;
#17801 = CARTESIAN_POINT ( 'NONE',  ( 3.209779917707810348, 11.89484142146541146, 6.673094556525186682 ) ) ;
#17802 = EDGE_CURVE ( 'NONE', #20069, #12648, #18952, .T. ) ;
#17803 = EDGE_CURVE ( 'NONE', #19273, #13378, #4586, .T. ) ;
#17804 = ORIENTED_EDGE ( 'NONE', *, *, #11225, .T. ) ;
#17805 = CARTESIAN_POINT ( 'NONE',  ( 49.15122309515935228, 34.52875999999999834, -25.07506492104907991 ) ) ;
#17806 = DIRECTION ( 'NONE',  ( -0.1060008583745224581, 0.000000000000000000, -0.9943660382494288186 ) ) ;
#17807 = CARTESIAN_POINT ( 'NONE',  ( 14.25617145423489696, -1.983739999999999393, -15.80779474975094168 ) ) ;
#17808 = DIRECTION ( 'NONE',  ( 1.000000000000000000, 0.000000000000000000, 0.000000000000000000 ) ) ;
#17809 = CARTESIAN_POINT ( 'NONE',  ( -21.43124999999999858, 32.54502000000000095, -4.860316984116058095E-16 ) ) ;
#17810 = ORIENTED_EDGE ( 'NONE', *, *, #16577, .T. ) ;
#17811 = VERTEX_POINT ( 'NONE', #21274 ) ;
#17812 = CARTESIAN_POINT ( 'NONE',  ( 10.78291357368954273, 17.61531206902142799, 7.284759546427739707 ) ) ;
#17814 = DIRECTION ( 'NONE',  ( 0.05085730733808142834, 0.000000000000000000, -0.9987059298363657467 ) ) ;
#17813 = DIRECTION ( 'NONE',  ( -0.4080888115384288528, 0.000000000000000000, -0.9129422336036122632 ) ) ;
#17815 = AXIS2_PLACEMENT_3D ( 'NONE', #8942, #9265, #19109 ) ;
#17816 = CARTESIAN_POINT ( 'NONE',  ( 12.91084050336935363, 11.37372653473270390, 4.572161392691734605 ) ) ;
#17817 = ORIENTED_EDGE ( 'NONE', *, *, #7822, .F. ) ;
#17818 = ORIENTED_EDGE ( 'NONE', *, *, #5715, .T. ) ;
#17819 = LINE ( 'NONE', #17701, #13465 ) ;
#17820 = CARTESIAN_POINT ( 'NONE',  ( 7.605715420845187147, 11.83137677356064721, -0.6597813618126635582 ) ) ;
#17821 = CARTESIAN_POINT ( 'NONE',  ( 3.737651886413042579, 15.57273015692113560, -0.6941798594830854707 ) ) ;
#17822 = CARTESIAN_POINT ( 'NONE',  ( 59.55063415577301811, 32.54502000000000095, -22.52230776719629191 ) ) ;
#17823 = CARTESIAN_POINT ( 'NONE',  ( 8.605384428358668458, 19.55736841712971952, 5.976435672814039535 ) ) ;
#17824 = VECTOR ( 'NONE', #16422, 1000.000000000000114 ) ;
#17825 = CARTESIAN_POINT ( 'NONE',  ( 7.183656975975698522, 13.24117894531195638, 6.480836668891950758 ) ) ;
#17826 = DIRECTION ( 'NONE',  ( -0.2868778675745011220, 0.000000000000000000, -0.9579671649362034858 ) ) ;
#17827 = CARTESIAN_POINT ( 'NONE',  ( 11.44137618178793936, 12.37556557019096282, -2.997012553075396823 ) ) ;
#17828 = CIRCLE ( 'NONE', #2641, 0.7950200000000005041 ) ;
#17829 = CARTESIAN_POINT ( 'NONE',  ( 13.65503668246327074, 22.05527566784187243, 1.855690361662355903 ) ) ;
#17830 = DIRECTION ( 'NONE',  ( 0.8609107660235850723, 0.000000000000000000, -0.5087559856598092844 ) ) ;
#17831 = CARTESIAN_POINT ( 'NONE',  ( -0.1175964564627289266, 17.37652828937785543, 0.04057638788381107142 ) ) ;
#17832 = CARTESIAN_POINT ( 'NONE',  ( 1.139206278029827768, 11.73021259349723167, 6.504762513190087247 ) ) ;
#17833 = EDGE_CURVE ( 'NONE', #374, #17763, #6732, .T. ) ;
#17834 = DIRECTION ( 'NONE',  ( 0.9636276526537417286, 0.000000000000000000, -0.2672484743474499158 ) ) ;
#17835 = CARTESIAN_POINT ( 'NONE',  ( 2.059594139655736900, 13.53433865536812064, 0.9666987378332712044 ) ) ;
#17836 = CARTESIAN_POINT ( 'NONE',  ( 53.09010322336158794, 40.07841907356969813, -16.72081503543966718 ) ) ;
#17837 = FACE_BOUND ( 'NONE', #9126, .T. ) ;
#17838 = CARTESIAN_POINT ( 'NONE',  ( 17.91249156466048831, -7.924689752748640181, -14.44214372066701735 ) ) ;
#17839 = AXIS2_PLACEMENT_3D ( 'NONE', #4307, #7514, #15934 ) ;
#17840 = EDGE_LOOP ( 'NONE', ( #13063, #20245, #14387, #615 ) ) ;
#17841 = CARTESIAN_POINT ( 'NONE',  ( 44.27024749654656688, 38.88803500000000213, -8.722764363618033201 ) ) ;
#17842 = CARTESIAN_POINT ( 'NONE',  ( 11.38874951053466233, 13.77064647055242652, 6.993025784648827070 ) ) ;
#17843 = VERTEX_POINT ( 'NONE', #12787 ) ;
#17844 = CARTESIAN_POINT ( 'NONE',  ( 29.21834112936799954, 1.789188963192005044, 10.70629397521275905 ) ) ;
#17845 = CARTESIAN_POINT ( 'NONE',  ( 5.498135393614799860, 17.47580698470410354, -2.050589633226200359 ) ) ;
#17846 = CARTESIAN_POINT ( 'NONE',  ( 26.59062499999999929, 30.16440499999999858, 8.335010000000000474 ) ) ;
#17847 = CARTESIAN_POINT ( 'NONE',  ( 1.495258403766146493, 14.30699635049795226, 8.420657258073232398 ) ) ;
#17848 = VERTEX_POINT ( 'NONE', #833 ) ;
#17849 = CYLINDRICAL_SURFACE ( 'NONE', #518, 2.381250000000001421 ) ;
#17850 = AXIS2_PLACEMENT_3D ( 'NONE', #14484, #21530, #11256 ) ;
#17851 = CARTESIAN_POINT ( 'NONE',  ( 9.648141209897488579, 17.23623480047593404, -3.067103124126105307 ) ) ;
#17852 = CARTESIAN_POINT ( 'NONE',  ( 65.90927232300019512, 0.000000000000000000, -12.91110117861467899 ) ) ;
#17853 = DIRECTION ( 'NONE',  ( -0.9579671649362032637, 0.000000000000000000, 0.2868778675745010664 ) ) ;
#17854 = EDGE_CURVE ( 'NONE', #21307, #2549, #14519, .T. ) ;
#17855 = CARTESIAN_POINT ( 'NONE',  ( 1.581041518826207248, -1.983739999999999393, -20.30277549736237575 ) ) ;
#17856 = DIRECTION ( 'NONE',  ( -0.4987171968201928873, 0.000000000000000000, 0.8667647648559606566 ) ) ;
#17857 = CARTESIAN_POINT ( 'NONE',  ( 4.562544981526344579, 20.60715472197122011, 6.559660940956183239 ) ) ;
#17858 = DIRECTION ( 'NONE',  ( 0.000000000000000000, 1.000000000000000000, 0.000000000000000000 ) ) ;
#17859 = ORIENTED_EDGE ( 'NONE', *, *, #2788, .F. ) ;
#17860 = CARTESIAN_POINT ( 'NONE',  ( -13.87568970999206108, 34.52875999999999834, -9.457638332870221376 ) ) ;
#17861 = DIRECTION ( 'NONE',  ( -0.08420877549337300871, 0.000000000000000000, -0.9964481331860212121 ) ) ;
#17862 = VERTEX_POINT ( 'NONE', #17757 ) ;
#17863 = CARTESIAN_POINT ( 'NONE',  ( 11.33566261673852793, 21.24491547887863163, 2.056737376786678784 ) ) ;
#17864 = CARTESIAN_POINT ( 'NONE',  ( 0.6175707511495683866, 19.59963610279798729, 7.191875376456732027 ) ) ;
#17865 = B_SPLINE_CURVE_WITH_KNOTS ( 'NONE', 3,
 ( #3130, #17958, #6451, #1253, #6225, #14663, #21474, #9855, #9982, #16312, #11316, #6118, #7993, #1351, #2806, #8095, #9540, #20024, #19703, #7888, #6331, #19817, #21369, #12997, #4576, #6559, #18066, #14767, #2928, #16624, #8215, #9654, #9755, #4690, #13214, #11434, #18179, #14988, #21703, #13320, #8645, #11967, #18811 ),
 .UNSPECIFIED., .F., .F.,
 ( 4, 3, 3, 3, 3, 3, 3, 3, 3, 3, 3, 3, 3, 3, 4 ),
 ( 0.000000000000000000, 0.09090909086281399876, 0.1818181817256480093, 0.2499255670981249955, 0.2727272725884720139, 0.3636363634512960186, 0.4545454543141200232, 0.4999095035919020047, 0.5454545451768439968, 0.6363636360396680569, 0.7272727269024920060, 0.7499460449993119449, 0.8181818177653160662, 0.9090909086281400153, 0.9999999994909640755 ),
 .UNSPECIFIED. ) ;
#17866 = CARTESIAN_POINT ( 'NONE',  ( 21.03152454542845717, -2.656576306117378827, -13.39494047124001952 ) ) ;
#17868 = CYLINDRICAL_SURFACE ( 'NONE', #9922, 0.7950200000000000600 ) ;
#17867 = CARTESIAN_POINT ( 'NONE',  ( 4.635270691011046829, 18.98716039713233883, 7.878850228405285705 ) ) ;
#17869 = ORIENTED_EDGE ( 'NONE', *, *, #1704, .F. ) ;
#17870 = SHAPE_REPRESENTATION_RELATIONSHIP ( 'NONE' , 'NONE' ,  #10883, #20091 ) ;
#17871 = CARTESIAN_POINT ( 'NONE',  ( 2.492193568723835462, -1.594802499999999013, -24.56873394466936134 ) ) ;
#17872 = CARTESIAN_POINT ( 'NONE',  ( 39.07402576619974610, -5.166360000000001840, -3.817946520901574825 ) ) ;
#17873 = ORIENTED_EDGE ( 'NONE', *, *, #4121, .F. ) ;
#17874 = CARTESIAN_POINT ( 'NONE',  ( 20.15758252994617550, -1.280876140752218895, -14.77588887141922847 ) ) ;
#17875 = CARTESIAN_POINT ( 'NONE',  ( 14.37725694972261081, 1.099222879083521676, -15.91397516589488781 ) ) ;
#17876 = ORIENTED_EDGE ( 'NONE', *, *, #8346, .F. ) ;
#17877 = CARTESIAN_POINT ( 'NONE',  ( 6.692329841978265748, 11.82482810032952081, 4.288276300720819556 ) ) ;
#17878 = CARTESIAN_POINT ( 'NONE',  ( 7.198342133457991565, 16.38025891712375781, -2.997146290384534506 ) ) ;
#17879 = EDGE_CURVE ( 'NONE', #9783, #17843, #13069, .T. ) ;
#17880 = EDGE_CURVE ( 'NONE', #16009, #18389, #2938, .T. ) ;
#17881 = CARTESIAN_POINT ( 'NONE',  ( 38.95212789349618987, -7.547369073570063591, -3.952970310398209897 ) ) ;
#17882 = VERTEX_POINT ( 'NONE', #19290 ) ;
#17883 = CARTESIAN_POINT ( 'NONE',  ( -13.49374999999999858, 30.56064500000000095, 0.000000000000000000 ) ) ;
#17884 = DIRECTION ( 'NONE',  ( -0.9987059298363656357, 0.000000000000000000, -0.05085730733808393328 ) ) ;
#17885 = ORIENTED_EDGE ( 'NONE', *, *, #1355, .F. ) ;
#17886 = ORIENTED_EDGE ( 'NONE', *, *, #1430, .T. ) ;
#17887 = CARTESIAN_POINT ( 'NONE',  ( 13.95408900351856119, 2.287844446565507450, -16.00547455423211574 ) ) ;
#17889 = DIRECTION ( 'NONE',  ( 1.000000000000000000, 0.000000000000000000, 0.000000000000000000 ) ) ;
#17888 = CARTESIAN_POINT ( 'NONE',  ( 5.026927007283006787, 11.34913591283086021, 5.616092169482095109 ) ) ;
#17890 = ORIENTED_EDGE ( 'NONE', *, *, #14597, .T. ) ;
#17891 = CARTESIAN_POINT ( 'NONE',  ( 3.796584004741204499, 12.36211805266656683, 0.3638733142846966029 ) ) ;
#17892 = EDGE_LOOP ( 'NONE', ( #12128, #14615, #15949, #14945 ) ) ;
#17893 = ORIENTED_EDGE ( 'NONE', *, *, #7640, .F. ) ;
#17894 = EDGE_CURVE ( 'NONE', #1735, #19311, #9988, .T. ) ;
#17895 = VECTOR ( 'NONE', #11058, 1000.000000000000000 ) ;
#17896 = ORIENTED_EDGE ( 'NONE', *, *, #16039, .T. ) ;
#17897 = EDGE_CURVE ( 'NONE', #2743, #17319, #21056, .T. ) ;
#17898 = CARTESIAN_POINT ( 'NONE',  ( 30.25543876212147509, 0.000000000000000000, -19.39939755251907272 ) ) ;
#17899 = CARTESIAN_POINT ( 'NONE',  ( 18.25624999999999787, 16.27314499999999953, 8.731249999999999289 ) ) ;
#17900 = CARTESIAN_POINT ( 'NONE',  ( -13.97426865170217702, -5.953760000000000829, -10.62412961436650249 ) ) ;
#17901 = CARTESIAN_POINT ( 'NONE',  ( -21.43124999999999858, 0.000000000000000000, -4.860316984116058095E-16 ) ) ;
#17902 = CARTESIAN_POINT ( 'NONE',  ( 3.395237882159598541, 12.51188876831191088, 7.527755607962313356 ) ) ;
#17903 = ORIENTED_EDGE ( 'NONE', *, *, #5876, .T. ) ;
#17904 = FACE_OUTER_BOUND ( 'NONE', #14637, .T. ) ;
#17905 = DIRECTION ( 'NONE',  ( 0.000000000000000000, 1.000000000000000000, 0.000000000000000000 ) ) ;
#17906 = FACE_OUTER_BOUND ( 'NONE', #16103, .T. ) ;
#17907 = CARTESIAN_POINT ( 'NONE',  ( 46.03750000000000142, 32.54502000000000095, -10.31874999999999964 ) ) ;
#17908 = EDGE_CURVE ( 'NONE', #16300, #6460, #21512, .T. ) ;
#17909 = B_SPLINE_CURVE_WITH_KNOTS ( 'NONE', 3,
 ( #5718, #2403, #6151, #17881, #19200 ),
 .UNSPECIFIED., .F., .F.,
 ( 4, 1, 4 ),
 ( 0.003754349818373690570, 0.003769101685636799468, 0.003783853552899908799 ),
 .UNSPECIFIED. ) ;
#17910 = ORIENTED_EDGE ( 'NONE', *, *, #8551, .T. ) ;
#17911 = ORIENTED_EDGE ( 'NONE', *, *, #1634, .F. ) ;
#17912 = CARTESIAN_POINT ( 'NONE',  ( 10.79087687479066382, 12.58417018233828166, -2.552037637521815228 ) ) ;
#17913 = AXIS2_PLACEMENT_3D ( 'NONE', #20203, #9716, #1636 ) ;
#17915 = DIRECTION ( 'NONE',  ( -0.9987059298363656357, 0.000000000000000000, -0.05085730733808393328 ) ) ;
#17914 = DIRECTION ( 'NONE',  ( 0.000000000000000000, 1.000000000000000000, 0.000000000000000000 ) ) ;
#17916 = CARTESIAN_POINT ( 'NONE',  ( 10.93549532874515329, 15.97885840934050883, -4.336554052330052755 ) ) ;
#17917 = ORIENTED_EDGE ( 'NONE', *, *, #9837, .F. ) ;
#17918 = ORIENTED_EDGE ( 'NONE', *, *, #3436, .F. ) ;
#17919 = DIRECTION ( 'NONE',  ( 0.7421532822901580895, -0.000000000000000000, -0.6702301885068630005 ) ) ;
#17920 = CARTESIAN_POINT ( 'NONE',  ( 8.468684176319758450, 21.29060048360308244, -0.02303094090340797664 ) ) ;
#17921 = EDGE_CURVE ( 'NONE', #12395, #21254, #18682, .T. ) ;
#17922 = CARTESIAN_POINT ( 'NONE',  ( 8.984891047036883904, 18.20044315508863519, 6.851887545445102923 ) ) ;
#17923 = CARTESIAN_POINT ( 'NONE',  ( 6.444640499250375854, 11.70121090254869145, 3.063182600979447390 ) ) ;
#17924 = EDGE_CURVE ( 'NONE', #10916, #6719, #4375, .T. ) ;
#17925 = EDGE_CURVE ( 'NONE', #13767, #13956, #10890, .T. ) ;
#17926 = AXIS2_PLACEMENT_3D ( 'NONE', #19535, #9359, #3958 ) ;
#17927 = CARTESIAN_POINT ( 'NONE',  ( 11.44907295303830352, 18.36121671486396778, -4.154917505379187581 ) ) ;
#17928 = CARTESIAN_POINT ( 'NONE',  ( 13.61114377367988837, 22.09400156900517942, 1.874518249454760088 ) ) ;
#17929 = LINE ( 'NONE', #6088, #20971 ) ;
#17930 = CARTESIAN_POINT ( 'NONE',  ( 42.35466991749225940, 34.52876000000000545, -17.94967221382040279 ) ) ;
#17931 = CARTESIAN_POINT ( 'NONE',  ( 3.234432283654637530, 11.90013693509636106, 6.894066948143128926 ) ) ;
#17932 = CARTESIAN_POINT ( 'NONE',  ( 1.141638631687549088, 11.73439853126398091, 6.515573991307596735 ) ) ;
#17933 = ORIENTED_EDGE ( 'NONE', *, *, #7404, .T. ) ;
#17934 = CARTESIAN_POINT ( 'NONE',  ( 1.414015556765540138, 13.15932452227622207, 7.490709649508223045 ) ) ;
#17935 = CARTESIAN_POINT ( 'NONE',  ( 35.47639361272155867, -6.752907499999998286, -41.40807265590733977 ) ) ;
#17936 = CARTESIAN_POINT ( 'NONE',  ( 39.16413618835606769, -1.983739999999999837, -24.45043885672975392 ) ) ;
#17937 = CARTESIAN_POINT ( 'NONE',  ( 19.97525939775061232, -6.161891578892464416, -14.01322510184426662 ) ) ;
#17938 = ORIENTED_EDGE ( 'NONE', *, *, #21197, .F. ) ;
#17939 = CARTESIAN_POINT ( 'NONE',  ( 53.25483508941461963, -9.531985000000000596, -5.879799058943532941 ) ) ;
#17940 = CARTESIAN_POINT ( 'NONE',  ( 10.38839620284240972, 21.50507767694745453, -0.5529639877510099666 ) ) ;
#17941 = ORIENTED_EDGE ( 'NONE', *, *, #20867, .T. ) ;
#17942 = CARTESIAN_POINT ( 'NONE',  ( 12.13621795668766445, -1.983739999999999393, 4.225309685850866082 ) ) ;
#17943 = CIRCLE ( 'NONE', #18294, 0.7950200000000003930 ) ;
#17944 = CARTESIAN_POINT ( 'NONE',  ( 5.803153002628106627, 19.17693049791878934, -1.408338056234150981 ) ) ;
#17945 = CARTESIAN_POINT ( 'NONE',  ( 66.03921914090641110, 0.000000000000000000, -10.93409647675949969 ) ) ;
#17946 = CARTESIAN_POINT ( 'NONE',  ( 6.097804090699195712, 20.44074137114568046, 5.245935090663635947 ) ) ;
#17947 = ORIENTED_EDGE ( 'NONE', *, *, #21078, .T. ) ;
#17948 = DIRECTION ( 'NONE',  ( -0.2490110332224850231, 0.000000000000000000, 0.9685006480810791629 ) ) ;
#17949 = EDGE_CURVE ( 'NONE', #19935, #11383, #7684, .T. ) ;
#17950 =( REPRESENTATION_RELATIONSHIP ('NONE','NONE', #15554, #17083 ) REPRESENTATION_RELATIONSHIP_WITH_TRANSFORMATION ( #10538 )SHAPE_REPRESENTATION_RELATIONSHIP( ) );
#17951 = LINE ( 'NONE', #1246, #19214 ) ;
#17952 = CARTESIAN_POINT ( 'NONE',  ( 12.96175805149838212, 21.47881914407666315, 0.4678899323171995528 ) ) ;
#17953 = DIRECTION ( 'NONE',  ( -0.6702301885068639997, 0.000000000000000000, -0.7421532822901570903 ) ) ;
#17954 = CARTESIAN_POINT ( 'NONE',  ( 8.505511374756364873, -6.752907499999998286, -20.97439202360551747 ) ) ;
#17955 = CARTESIAN_POINT ( 'NONE',  ( 0.3048720416742233819, 19.02512202735066182, 0.6306780995777144794 ) ) ;
#17956 = DIRECTION ( 'NONE',  ( 0.2490110332224850509, 0.000000000000000000, -0.9685006480810792739 ) ) ;
#17957 = AXIS2_PLACEMENT_3D ( 'NONE', #895, #9066, #18909 ) ;
#17958 = CARTESIAN_POINT ( 'NONE',  ( 6.432178468024032369, 11.71523184318539279, 2.836886883351238176 ) ) ;
#17959 = CARTESIAN_POINT ( 'NONE',  ( 59.90456643211351917, 34.52875999999999834, -2.926035437812116946 ) ) ;
#17960 = PLANE ( 'NONE',  #422 ) ;
#17961 = DIRECTION ( 'NONE',  ( 1.000000000000000000, 0.000000000000000000, 0.000000000000000000 ) ) ;
#17962 = EDGE_CURVE ( 'NONE', #14925, #3318, #9148, .T. ) ;
#17963 = ORIENTED_EDGE ( 'NONE', *, *, #13193, .F. ) ;
#17964 = CARTESIAN_POINT ( 'NONE',  ( -6.268352501591477832, -0.7997824999999986195, -35.49402737582407497 ) ) ;
#17965 = DIRECTION ( 'NONE',  ( 0.000000000000000000, 1.000000000000000000, 0.000000000000000000 ) ) ;
#17966 = ORIENTED_EDGE ( 'NONE', *, *, #597, .T. ) ;
#17967 = CARTESIAN_POINT ( 'NONE',  ( 10.68594047828121418, 21.00681492881632195, 0.3047970212069722740 ) ) ;
#17968 = CARTESIAN_POINT ( 'NONE',  ( 1.484066998577597385, 15.20418130093746001, 8.701018632067329506 ) ) ;
#17969 = CARTESIAN_POINT ( 'NONE',  ( 21.28779318124766107, -2.646397705288468405, -13.84543864803846880 ) ) ;
#17971 = DIRECTION ( 'NONE',  ( 0.000000000000000000, 1.000000000000000000, -0.000000000000000000 ) ) ;
#17970 = CARTESIAN_POINT ( 'NONE',  ( 0.4657302212947604381, 12.03899270364792073, 4.948057704354145159 ) ) ;
#17972 = ORIENTED_EDGE ( 'NONE', *, *, #6381, .F. ) ;
#17973 = CARTESIAN_POINT ( 'NONE',  ( -12.58923395807689616, -0.3962399999999990929, -0.9319226134156148866 ) ) ;
#17974 = EDGE_CURVE ( 'NONE', #1074, #13360, #8225, .T. ) ;
#17975 = VERTEX_POINT ( 'NONE', #21602 ) ;
#17976 = CARTESIAN_POINT ( 'NONE',  ( 19.50266732720887219, -0.07610042702671838966, -15.00324811268347602 ) ) ;
#17977 = B_SPLINE_SURFACE_WITH_KNOTS ( 'NONE', 3, 3, ( 
 ( #7276, #14037, #20742, #2292, #20851, #7377, #14149, #3515, #5724, #194, #6936, #2813, #5692, #7679, #5809, #12665, #21156, #12783, #19506 ),
 ( #16526, #15096, #11538, #1160, #10486, #7899, #6132, #5500, #7285, #4482, #3858, #12371, #17969, #17457, #13011, #2070, #19715, #15588, #19098 ),
 ( #10596, #20755, #18985, #12262, #12903, #19512, #7178, #17343, #2300, #14445, #17227, #19615, #2191, #21276, #13943, #8932, #21384, #7388, #20640 ),
 ( #16322, #11218, #4380, #3967, #21162, #6017, #8811, #12789, #2711, #14676, #11114, #15709, #17866, #9445, #2819, #9554, #537, #14047, #16217 ),
 ( #1044, #7789, #5611, #14557, #10712, #9037, #638, #15812, #19939, #21487, #3043, #13229, #8007, #5016, #18079, #21717, #14778, #15102, #1591 ),
 ( #14884, #11545, #4587, #11329, #3259, #2939, #21603, #18283, #11653, #3144, #30, #4903, #10100, #9868, #6570, #6343, #11771, #9995, #8333 ),
 ( #6669, #1264, #6465, #1687, #18387, #4812, #21816, #13543, #15001, #6782, #16750, #8426, #9768, #16534, #18496, #16847, #1364, #9664, #15202 ),
 ( #8107, #13430, #16636, #16433, #11445, #13117, #3368, #13332, #20141, #19830, #4705, #18190, #1479, #20034, #8226, #484, #17282, #13764, #5332 ),
 ( #17407, #17172, #5553, #3469, #13652, #3689, #2012, #6891, #10203, #12310, #15762, #8653, #20353, #5222, #20464, #5124, #7237, #18602, #13995 ) ),
 .UNSPECIFIED., .F., .F., .F.,
 ( 4, 1, 1, 1, 1, 1, 4 ),
 ( 4, 1, 1, 1, 1, 1, 1, 1, 1, 1, 1, 1, 1, 1, 1, 1, 4 ),
 ( 0.4864838642302999894, 0.5000000000000000000, 0.6250000000000000000, 0.7500000000000000000, 0.8750000000000000000, 1.000000000000000000, 1.013516135769999993 ),
 ( -0.02000001207767999889, 0.04500002717478000097, 0.1100000664272000050, 0.1750001056797000076, 0.2400001449321000069, 0.3050001841846000095, 0.3700002234370000087, 0.4350002626895000390, 0.5000003019419000383, 0.5650003411944000131, 0.6300003804468999880, 0.6950004196992999317, 0.7600004589518000175, 0.8250004982041999613, 0.8900005374567000471, 0.9550005767090999909, 1.020000615962000090 ),
 .UNSPECIFIED. ) ;
#17978 = ORIENTED_EDGE ( 'NONE', *, *, #10600, .T. ) ;
#17979 = CARTESIAN_POINT ( 'NONE',  ( 9.159028214282953329, 13.35013903698374094, 6.344229879298691088 ) ) ;
#17980 = CARTESIAN_POINT ( 'NONE',  ( 9.450995817226065299, 19.32892518063468046, -2.971067605327898598 ) ) ;
#17981 = CARTESIAN_POINT ( 'NONE',  ( 19.65195596176846848, -4.944832552674430559, -15.35560206351170898 ) ) ;
#17982 = DIRECTION ( 'NONE',  ( -0.2868778675745011220, 0.000000000000000000, -0.9579671649362034858 ) ) ;
#17983 = CIRCLE ( 'NONE', #20075, 1.785937499999998179 ) ;
#17984 = ORIENTED_EDGE ( 'NONE', *, *, #11479, .F. ) ;
#17985 = DIRECTION ( 'NONE',  ( 0.000000000000000000, 1.000000000000000000, 0.000000000000000000 ) ) ;
#17986 = ORIENTED_EDGE ( 'NONE', *, *, #4111, .F. ) ;
#17987 = ORIENTED_EDGE ( 'NONE', *, *, #19137, .T. ) ;
#17988 = LINE ( 'NONE', #958, #11671 ) ;
#17990 = DIRECTION ( 'NONE',  ( 0.000000000000000000, -1.000000000000000000, -0.000000000000000000 ) ) ;
#17989 = CARTESIAN_POINT ( 'NONE',  ( 2.914188686793144800, 19.78346126529704208, 8.029142585942892651 ) ) ;
#17991 = EDGE_LOOP ( 'NONE', ( #8958, #13273, #14361, #8623 ) ) ;
#17992 = CARTESIAN_POINT ( 'NONE',  ( 3.514438851728853397, 15.55170815036052367, -1.360445981688413353 ) ) ;
#17993 = CIRCLE ( 'NONE', #16924, 1.190625000000001155 ) ;
#17994 = ORIENTED_EDGE ( 'NONE', *, *, #13022, .T. ) ;
#17995 = EDGE_CURVE ( 'NONE', #18464, #3406, #10949, .T. ) ;
#17996 = ORIENTED_EDGE ( 'NONE', *, *, #2193, .T. ) ;
#17997 = ORIENTED_EDGE ( 'NONE', *, *, #18597, .T. ) ;
#17998 = CARTESIAN_POINT ( 'NONE',  ( 4.210488876653085022, 12.18174440138109027, 2.120801485575080303 ) ) ;
#17999 = CIRCLE ( 'NONE', #2102, 3.174999999999997158 ) ;
#18000 = DIRECTION ( 'NONE',  ( 0.000000000000000000, 1.000000000000000000, 0.000000000000000000 ) ) ;
#18001 = CARTESIAN_POINT ( 'NONE',  ( 29.19635173153840313, 32.54502000000000095, -6.218966092919240296 ) ) ;
#18002 = CARTESIAN_POINT ( 'NONE',  ( 1.923689137428217455, -0.9589899600121986056, -20.61772871637841220 ) ) ;
#18003 = CARTESIAN_POINT ( 'NONE',  ( 65.90927232300019512, 1.984375000000000000, -12.91110117861467899 ) ) ;
#18004 = CARTESIAN_POINT ( 'NONE',  ( 3.642626662481108557, 14.63523096079658181, 8.921394353827624357 ) ) ;
#18005 = EDGE_LOOP ( 'NONE', ( #4696, #400 ) ) ;
#18006 = CARTESIAN_POINT ( 'NONE',  ( -22.70813868260604096, 0.000000000000000000, 1.090609736204201763 ) ) ;
#18007 = CARTESIAN_POINT ( 'NONE',  ( 1.532169971477637782, 5.548947500000001476, -20.71839214105750315 ) ) ;
#18008 = CARTESIAN_POINT ( 'NONE',  ( -23.01875000000000071, 1.984375000000000000, -10.31874999999999964 ) ) ;
#18009 = CARTESIAN_POINT ( 'NONE',  ( -16.07247711516169275, 37.85422182005619618, -10.44681224123558039 ) ) ;
#18010 = EDGE_CURVE ( 'NONE', #13909, #17126, #13227, .T. ) ;
#18011 = DIRECTION ( 'NONE',  ( 0.9129422336036140395, 0.000000000000000000, -0.4080888115384250225 ) ) ;
#18012 = ORIENTED_EDGE ( 'NONE', *, *, #10925, .T. ) ;
#18013 = ORIENTED_EDGE ( 'NONE', *, *, #12771, .T. ) ;
#18014 = CARTESIAN_POINT ( 'NONE',  ( 9.052293558324171485, 17.23623480047593404, -2.888667463761888765 ) ) ;
#18015 = MECHANICAL_DESIGN_GEOMETRIC_PRESENTATION_REPRESENTATION (  '', ( #15567 ), #1058 ) ;
#18017 = DIRECTION ( 'NONE',  ( -0.7421532822901580895, 0.000000000000000000, 0.6702301885068630005 ) ) ;
#18016 = CARTESIAN_POINT ( 'NONE',  ( 39.62791084302666178, 32.54502000000000095, -24.65774797299118859 ) ) ;
#18018 = CARTESIAN_POINT ( 'NONE',  ( 12.32999047502645773, 21.73372772506127149, -1.020500756129577580 ) ) ;
#18019 = VERTEX_POINT ( 'NONE', #19937 ) ;
#18020 = ORIENTED_EDGE ( 'NONE', *, *, #11699, .T. ) ;
#18021 = CARTESIAN_POINT ( 'NONE',  ( 4.936390548048069427, -1.594802499999999013, -19.84313358055101517 ) ) ;
#18022 = EDGE_CURVE ( 'NONE', #13041, #6616, #8798, .T. ) ;
#18023 = ADVANCED_FACE ( 'NONE', ( #3662, #11542 ), #10407, .T. ) ;
#18024 = EDGE_CURVE ( 'NONE', #18743, #19312, #17999, .T. ) ;
#18025 = AXIS2_PLACEMENT_3D ( 'NONE', #12300, #12419, #15754 ) ;
#18026 = CARTESIAN_POINT ( 'NONE',  ( 8.548988628242938148, 19.70142182889846794, 5.837084678231597934 ) ) ;
#18027 = FACE_OUTER_BOUND ( 'NONE', #9003, .T. ) ;
#18028 = VECTOR ( 'NONE', #3201, 1000.000000000000227 ) ;
#18029 = CARTESIAN_POINT ( 'NONE',  ( 13.76432530034137613, 21.82393085918102571, 1.789009612944968186 ) ) ;
#18030 = CARTESIAN_POINT ( 'NONE',  ( -17.46249999999999858, 34.31794000000000011, 0.000000000000000000 ) ) ;
#18031 = DIRECTION ( 'NONE',  ( 0.000000000000000000, -1.000000000000000000, -0.000000000000000000 ) ) ;
#18032 = CARTESIAN_POINT ( 'NONE',  ( 2.439682189296471737, 11.21420404894608147, 3.451098197904673093 ) ) ;
#18033 = CARTESIAN_POINT ( 'NONE',  ( 1.413168230598596864, 12.44285152367415748, 7.753309353558566208 ) ) ;
#18034 = DIRECTION ( 'NONE',  ( 0.000000000000000000, -1.000000000000000000, -0.000000000000000000 ) ) ;
#18035 = VERTEX_POINT ( 'NONE', #11650 ) ;
#18036 = CIRCLE ( 'NONE', #1780, 20.83593750000000000 ) ;
#18037 = CARTESIAN_POINT ( 'NONE',  ( 3.230455007503029830, 12.59595915030716284, 6.454679934702889810 ) ) ;
#18038 = DIRECTION ( 'NONE',  ( 0.000000000000000000, 1.000000000000000000, 0.000000000000000000 ) ) ;
#18039 = DIRECTION ( 'NONE',  ( 0.000000000000000000, 1.000000000000000000, 0.000000000000000000 ) ) ;
#18040 = CARTESIAN_POINT ( 'NONE',  ( 14.51424632332418163, -8.292823964279493865, -15.18575921541595974 ) ) ;
#18041 = ADVANCED_FACE ( 'NONE', ( #8004 ), #15099, .T. ) ;
#18042 = VERTEX_POINT ( 'NONE', #6569 ) ;
#18043 = CARTESIAN_POINT ( 'NONE',  ( -21.34815828341188393, 0.000000000000000000, 0.8078590638549643099 ) ) ;
#18044 = CARTESIAN_POINT ( 'NONE',  ( 7.124527213025964478, 16.38034437524489206, -2.979516426361350057 ) ) ;
#18045 = CARTESIAN_POINT ( 'NONE',  ( 9.276037966993236239, 18.10005428927824767, -3.373736345999344799 ) ) ;
#18046 = ORIENTED_EDGE ( 'NONE', *, *, #17426, .F. ) ;
#18047 = AXIS2_PLACEMENT_3D ( 'NONE', #21722, #15004, #34 ) ;
#18048 = CARTESIAN_POINT ( 'NONE',  ( 27.23577668703720178, 1.270868477333907842, 10.58329832977197960 ) ) ;
#18049 = AXIS2_PLACEMENT_3D ( 'NONE', #16221, #21387, #16111 ) ;
#18050 = CARTESIAN_POINT ( 'NONE',  ( 6.295715859104048739, 20.62233829775750138, -0.1650162826167260732 ) ) ;
#18051 = FACE_OUTER_BOUND ( 'NONE', #21296, .T. ) ;
#18052 = CARTESIAN_POINT ( 'NONE',  ( 5.302404883823700565, 15.73838188847654784, 8.113367678063646338 ) ) ;
#18053 = EDGE_CURVE ( 'NONE', #13084, #13225, #5280, .T. ) ;
#18054 = AXIS2_PLACEMENT_3D ( 'NONE', #9691, #21846, #18420 ) ;
#18055 = CARTESIAN_POINT ( 'NONE',  ( 54.11611804786240043, 1.984375000000000000, -30.58983753981140197 ) ) ;
#18056 = CARTESIAN_POINT ( 'NONE',  ( -29.36874999999999858, 0.000000000000000000, -3.968750000000000000 ) ) ;
#18057 = CARTESIAN_POINT ( 'NONE',  ( 11.60913865796776712, 21.44411105555546015, 1.903085412513896291 ) ) ;
#18058 = CARTESIAN_POINT ( 'NONE',  ( 5.249757807197408255, 17.14787612431637598, 7.964819928734911514 ) ) ;
#18059 = AXIS2_PLACEMENT_3D ( 'NONE', #5785, #12543, #19268 ) ;
#18060 = PLANE ( 'NONE',  #6121 ) ;
#18061 = DIRECTION ( 'NONE',  ( -0.2672484743474500268, 0.000000000000000000, -0.9636276526537417286 ) ) ;
#18062 = CARTESIAN_POINT ( 'NONE',  ( 6.572371458150938039, 21.10281604008488188, 5.417636278889840007 ) ) ;
#18063 = CARTESIAN_POINT ( 'NONE',  ( 31.68988926855799448, -1.983739999999999837, 1.626235259850384418 ) ) ;
#18064 = AXIS2_PLACEMENT_3D ( 'NONE', #8839, #3773, #3659 ) ;
#18065 = CARTESIAN_POINT ( 'NONE',  ( 39.11079947626275555, 34.52875999999999834, -27.65534212225540500 ) ) ;
#18066 = CARTESIAN_POINT ( 'NONE',  ( 6.745904810994247214, 11.18924887071056240, 2.704525624254954685 ) ) ;
#18067 = CARTESIAN_POINT ( 'NONE',  ( 49.16323787629939801, 32.54502000000000095, -27.09503225884920141 ) ) ;
#18068 = CARTESIAN_POINT ( 'NONE',  ( 22.04181838752732148, 16.26393749999999727, 0.06645525512612464325 ) ) ;
#18069 = EDGE_CURVE ( 'NONE', #19957, #11624, #20033, .T. ) ;
#18070 = EDGE_CURVE ( 'NONE', #1480, #5927, #6351, .T. ) ;
#18071 = CARTESIAN_POINT ( 'NONE',  ( -3.037751992662818257, 26.98019749999999917, -30.02724401157551526 ) ) ;
#18072 = AXIS2_PLACEMENT_3D ( 'NONE', #11840, #3540, #21677 ) ;
#18073 = EDGE_LOOP ( 'NONE', ( #21735, #803, #19989, #18718, #6269 ) ) ;
#18074 = DIRECTION ( 'NONE',  ( 0.9173788132826626862, 0.000000000000000000, -0.3980152169705242216 ) ) ;
#18075 = CARTESIAN_POINT ( 'NONE',  ( 21.43124999999999858, 16.27314499999999953, 10.71562499999999929 ) ) ;
#18076 = VERTEX_POINT ( 'NONE', #3041 ) ;
#18077 = CARTESIAN_POINT ( 'NONE',  ( 10.36704172787692890, 20.61404234333509322, -0.5420488695692129433 ) ) ;
#18078 = DIRECTION ( 'NONE',  ( 0.2490110332224848289, 0.000000000000000000, -0.9685006480810792739 ) ) ;
#18079 = CARTESIAN_POINT ( 'NONE',  ( 17.52900673049509805, -7.713162168938938024, -13.85515164265490462 ) ) ;
#18080 = FACE_OUTER_BOUND ( 'NONE', #21596, .T. ) ;
#18081 = ORIENTED_EDGE ( 'NONE', *, *, #12249, .T. ) ;
#18082 = DIRECTION ( 'NONE',  ( 0.000000000000000000, 1.000000000000000000, 0.000000000000000000 ) ) ;
#18083 = AXIS2_PLACEMENT_3D ( 'NONE', #3758, #14374, #20993 ) ;
#18084 = VECTOR ( 'NONE', #4453, 1000.000000000000000 ) ;
#18085 = VECTOR ( 'NONE', #17125, 1000.000000000000000 ) ;
#18086 = ORIENTED_EDGE ( 'NONE', *, *, #10629, .T. ) ;
#18087 = CARTESIAN_POINT ( 'NONE',  ( 19.83216830577377365, -0.7115147061423999775, -14.88007337591235846 ) ) ;
#18088 = CARTESIAN_POINT ( 'NONE',  ( 0.7153167063906088474, 19.36228057343206999, 2.036841758829455618 ) ) ;
#18089 = VECTOR ( 'NONE', #3739, 1000.000000000000114 ) ;
#18090 = ORIENTED_EDGE ( 'NONE', *, *, #2912, .F. ) ;
#18091 = CIRCLE ( 'NONE', #4676, 0.7950199999999982836 ) ;
#18092 = CARTESIAN_POINT ( 'NONE',  ( 6.801299041159860614, 12.02528521847468213, 4.783667443132798347 ) ) ;
#18093 = CARTESIAN_POINT ( 'NONE',  ( 38.36471077000297925, 38.15731773671534910, -4.673719963191772742 ) ) ;
#18094 = CARTESIAN_POINT ( 'NONE',  ( 6.465162621008090582, 10.79737175431668206, 3.234340088657999601 ) ) ;
#18095 = AXIS2_PLACEMENT_3D ( 'NONE', #6714, #13470, #5255 ) ;
#18096 = CARTESIAN_POINT ( 'NONE',  ( 19.18622267977934470, -5.669706517139640134, -15.43468797119958502 ) ) ;
#18097 = EDGE_CURVE ( 'NONE', #5953, #17848, #1051, .T. ) ;
#18098 = DIRECTION ( 'NONE',  ( 1.000000000000000000, 0.000000000000000000, 0.000000000000000000 ) ) ;
#18099 = EDGE_LOOP ( 'NONE', ( #9513, #21511, #2718, #18383 ) ) ;
#18100 = LINE ( 'NONE', #2959, #14978 ) ;
#18101 = CARTESIAN_POINT ( 'NONE',  ( 53.14266576735298031, -7.546379553159687781, -16.66242751532464084 ) ) ;
#18102 = ORIENTED_EDGE ( 'NONE', *, *, #5294, .F. ) ;
#18103 = ORIENTED_EDGE ( 'NONE', *, *, #6811, .T. ) ;
#18104 = AXIS2_PLACEMENT_3D ( 'NONE', #14018, #12337, #10683 ) ;
#18105 = CYLINDRICAL_SURFACE ( 'NONE', #15221, 2.182812499999999378 ) ;
#18106 = AXIS2_PLACEMENT_3D ( 'NONE', #625, #4164, #7369 ) ;
#18108 = CARTESIAN_POINT ( 'NONE',  ( 60.38511073144201191, 32.54502000000000095, -22.26373525985038526 ) ) ;
#18107 = CARTESIAN_POINT ( 'NONE',  ( 7.434093443094676346, 16.64415285869171868, 8.524580364682270428 ) ) ;
#18109 = ORIENTED_EDGE ( 'NONE', *, *, #19537, .F. ) ;
#18110 = CARTESIAN_POINT ( 'NONE',  ( 3.583776055977702324, 13.69441953482172636, -0.7122204557510644074 ) ) ;
#18111 = VERTEX_POINT ( 'NONE', #6667 ) ;
#18112 = VERTEX_POINT ( 'NONE', #13428 ) ;
#18113 = CARTESIAN_POINT ( 'NONE',  ( 0.9676402247297362091, 12.33599599044877237, 5.805161455712580576 ) ) ;
#18114 = AXIS2_PLACEMENT_3D ( 'NONE', #11592, #80, #1627 ) ;
#18115 = VERTEX_POINT ( 'NONE', #16531 ) ;
#18116 = CARTESIAN_POINT ( 'NONE',  ( 2.277511255392748790, 12.44482274936954624, 2.512107328279189034 ) ) ;
#18117 = AXIS2_PLACEMENT_3D ( 'NONE', #18485, #5112, #11860 ) ;
#18118 = DIRECTION ( 'NONE',  ( -0.3482992169606098365, 0.9330960544336215357, -0.08955115110948595747 ) ) ;
#18119 = LINE ( 'NONE', #874, #6156 ) ;
#18120 = LINE ( 'NONE', #971, #6503 ) ;
#18121 = DIRECTION ( 'NONE',  ( 0.9876802608827760510, 0.000000000000000000, -0.1564854698127960131 ) ) ;
#18122 = CARTESIAN_POINT ( 'NONE',  ( 2.639050747364091176, 11.24676862501781294, 4.183082657504865409 ) ) ;
#18123 = EDGE_CURVE ( 'NONE', #14487, #14185, #19399, .T. ) ;
#18124 = ORIENTED_EDGE ( 'NONE', *, *, #19528, .T. ) ;
#18125 = CARTESIAN_POINT ( 'NONE',  ( -18.18961309330695997, 35.81157980123359863, -25.80119252674831998 ) ) ;
#18126 = LINE ( 'NONE', #10934, #19838 ) ;
#18127 = DIRECTION ( 'NONE',  ( -0.9579671649362032637, 0.000000000000000000, 0.2868778675745013440 ) ) ;
#18128 = CARTESIAN_POINT ( 'NONE',  ( 53.31277592387545639, 40.04741288645178088, -16.46826747127406421 ) ) ;
#18129 = AXIS2_PLACEMENT_3D ( 'NONE', #17215, #2058, #5599 ) ;
#18130 = EDGE_LOOP ( 'NONE', ( #952, #18983, #3632, #3046 ) ) ;
#18131 = ORIENTED_EDGE ( 'NONE', *, *, #17626, .T. ) ;
#18132 = CARTESIAN_POINT ( 'NONE',  ( 5.360055287488979303, 17.26127046106770635, -1.409361485115639523 ) ) ;
#18133 = CARTESIAN_POINT ( 'NONE',  ( 54.55586098912687731, -9.531985000000000596, -6.056925149195119040 ) ) ;
#18134 = CARTESIAN_POINT ( 'NONE',  ( 11.49570108219309716, 19.89147748586559317, -3.243642535669593929 ) ) ;
#18135 = EDGE_LOOP ( 'NONE', ( #12369, #8060, #530, #17789 ) ) ;
#18136 = ORIENTED_EDGE ( 'NONE', *, *, #2643, .F. ) ;
#18137 = DIRECTION ( 'NONE',  ( 0.000000000000000000, 0.000000000000000000, 1.000000000000000000 ) ) ;
#18138 = B_SPLINE_CURVE_WITH_KNOTS ( 'NONE', 3,
 ( #3814, #3184, #11481, #17296, #499 ),
 .UNSPECIFIED., .F., .F.,
 ( 4, 1, 4 ),
 ( 0.000000000000000000, 2.695145556491273853E-05, 5.390291112982547705E-05 ),
 .UNSPECIFIED. ) ;
#18139 = CARTESIAN_POINT ( 'NONE',  ( 8.916212456033903777, 12.27243947381834666, 5.041701324839980458 ) ) ;
#18140 = B_SPLINE_CURVE_WITH_KNOTS ( 'NONE', 3,
 ( #9050, #17364, #14174, #10728, #654, #7400, #2431, #15939, #767, #7518 ),
 .UNSPECIFIED., .F., .F.,
 ( 4, 2, 2, 2, 4 ),
 ( 0.000000000000000000, 0.2500000000000000000, 0.5000000000000000000, 0.7500000000000000000, 1.000000000000000000 ),
 .UNSPECIFIED. ) ;
#18141 = CARTESIAN_POINT ( 'NONE',  ( 3.372867663120830528, 16.47655830875484639, 8.442787653594567843 ) ) ;
#18142 = EDGE_CURVE ( 'NONE', #6968, #6063, #6698, .T. ) ;
#18143 = AXIS2_PLACEMENT_3D ( 'NONE', #2201, #12599, #14056 ) ;
#18144 = PLANE ( 'NONE',  #5265 ) ;
#18145 = CARTESIAN_POINT ( 'NONE',  ( 13.55239428341091212, 21.42532649923676402, 1.793975647907078308 ) ) ;
#18146 = CARTESIAN_POINT ( 'NONE',  ( 11.42842559562532578, -3.968114999999999615, 1.673196738795719174 ) ) ;
#18147 = CARTESIAN_POINT ( 'NONE',  ( 4.560374023055850046, 10.97171856713620031, 3.825589676116931681 ) ) ;
#18148 = CARTESIAN_POINT ( 'NONE',  ( 1.580932918030141687, 13.29898186247538838, 8.589096705807090615 ) ) ;
#18149 = EDGE_CURVE ( 'NONE', #8377, #7695, #5646, .T. ) ;
#18150 = CYLINDRICAL_SURFACE ( 'NONE', #19672, 1.984375000000000000 ) ;
#18151 = EDGE_CURVE ( 'NONE', #5739, #11489, #9854, .T. ) ;
#18152 = VERTEX_POINT ( 'NONE', #17930 ) ;
#18153 = CARTESIAN_POINT ( 'NONE',  ( 0.9039476154303529576, 19.66626656054290123, 2.236627047933878121 ) ) ;
#18154 = AXIS2_PLACEMENT_3D ( 'NONE', #18030, #2676, #21670 ) ;
#18155 = DIRECTION ( 'NONE',  ( -1.000000000000000000, 0.000000000000000000, 0.000000000000000000 ) ) ;
#18156 = DIRECTION ( 'NONE',  ( -0.9685006480810791629, 0.000000000000000000, -0.2490110332224850509 ) ) ;
#18157 = CARTESIAN_POINT ( 'NONE',  ( 19.61169252880100089, -6.639328201340718216, -14.08464967305818938 ) ) ;
#18158 = ORIENTED_EDGE ( 'NONE', *, *, #5324, .T. ) ;
#18159 = CARTESIAN_POINT ( 'NONE',  ( 8.781357490942916399, 40.07707250000000698, -18.85455479843708559 ) ) ;
#18160 = CARTESIAN_POINT ( 'NONE',  ( 14.04250245428990951, 21.64281653910636294, 3.683363989245958869 ) ) ;
#18161 = DIRECTION ( 'NONE',  ( -0.9685006480810791629, 0.000000000000000000, -0.2490110332224850231 ) ) ;
#18162 = CARTESIAN_POINT ( 'NONE',  ( 9.219858665001117615, 17.68564764128002409, -3.478853225350395650 ) ) ;
#18163 = ORIENTED_EDGE ( 'NONE', *, *, #15908, .F. ) ;
#18164 = VECTOR ( 'NONE', #16252, 1000.000000000000000 ) ;
#18165 = PRODUCT ( 'Ratchet Main Fixed Frame', 'Ratchet Main Fixed Frame', '', ( #10657 ) ) ;
#18166 = CARTESIAN_POINT ( 'NONE',  ( 7.157577278382974306, 21.65757474929394277, 2.163353812009434218 ) ) ;
#18167 = DIRECTION ( 'NONE',  ( 1.000000000000000000, 0.000000000000000000, 0.000000000000000000 ) ) ;
#18168 = CARTESIAN_POINT ( 'NONE',  ( 3.206323496511946480, 17.96108129601270775, 8.216359125560503074 ) ) ;
#18169 = DIRECTION ( 'NONE',  ( 0.000000000000000000, 1.000000000000000000, 0.000000000000000000 ) ) ;
#18170 = DIRECTION ( 'NONE',  ( -0.9685006480810793850, 0.000000000000000000, -0.2490110332224846623 ) ) ;
#18171 = CIRCLE ( 'NONE', #16071, 19.05000000000000071 ) ;
#18172 = EDGE_CURVE ( 'NONE', #10096, #3095, #14480, .T. ) ;
#18173 = CARTESIAN_POINT ( 'NONE',  ( 13.45774086459438479, 16.70784808449734982, 6.497954125047418650 ) ) ;
#18174 = VECTOR ( 'NONE', #18374, 1000.000000000000000 ) ;
#18175 = CARTESIAN_POINT ( 'NONE',  ( 1.957410110268193559, 21.29427857361828202, 4.965368193760166804 ) ) ;
#18176 = CARTESIAN_POINT ( 'NONE',  ( 61.65536943582333151, 32.54502000000000095, -11.98363747855214712 ) ) ;
#18177 = EDGE_CURVE ( 'NONE', #20882, #21748, #19353, .T. ) ;
#18178 = CARTESIAN_POINT ( 'NONE',  ( 51.69314645384351081, -6.356984999999999886, -17.03058447914853346 ) ) ;
#18179 = CARTESIAN_POINT ( 'NONE',  ( 6.586735130854707521, 10.98645991353044238, 2.737382233163811573 ) ) ;
#18180 = CARTESIAN_POINT ( 'NONE',  ( 39.11418302930122337, 40.08456717457784890, -3.775083184656583768 ) ) ;
#18181 = CARTESIAN_POINT ( 'NONE',  ( 19.76333778421562215, -6.796690732811715208, -15.26778210143417702 ) ) ;
#18182 = LINE ( 'NONE', #3134, #13802 ) ;
#18183 = ORIENTED_EDGE ( 'NONE', *, *, #6158, .F. ) ;
#18184 = FACE_OUTER_BOUND ( 'NONE', #4593, .T. ) ;
#18185 = DIRECTION ( 'NONE',  ( -0.7421532822901579785, 0.000000000000000000, 0.6702301885068630005 ) ) ;
#18186 = ORIENTED_EDGE ( 'NONE', *, *, #620, .T. ) ;
#18187 = CARTESIAN_POINT ( 'NONE',  ( 9.483053905913827464, 17.79016367847964375, -2.669168664533136948 ) ) ;
#18188 = DIRECTION ( 'NONE',  ( 0.000000000000000000, 1.000000000000000000, 0.000000000000000000 ) ) ;
#18189 = CARTESIAN_POINT ( 'NONE',  ( 52.19854938732527216, 38.72945808962413849, -17.58284632693144189 ) ) ;
#18190 = CARTESIAN_POINT ( 'NONE',  ( 19.12285863748637382, -0.2473773731819471633, -14.52246859281454761 ) ) ;
#18191 = CARTESIAN_POINT ( 'NONE',  ( 50.29383871662588490, -4.569743463999999200, -28.02957329025317179 ) ) ;
#18192 = VERTEX_POINT ( 'NONE', #11282 ) ;
#18193 =( NAMED_UNIT ( * ) PLANE_ANGLE_UNIT ( ) SI_UNIT ( $, .RADIAN. ) );
#18194 = CIRCLE ( 'NONE', #12180, 0.3962399999999975386 ) ;
#18195 = DIRECTION ( 'NONE',  ( 0.9790635044817342925, 0.000000000000000000, -0.2035550397114870569 ) ) ;
#18196 = ORIENTED_EDGE ( 'NONE', *, *, #8436, .F. ) ;
#18197 = CARTESIAN_POINT ( 'NONE',  ( 19.43379288100138069, 0.07459186394039191148, -15.02802818531180584 ) ) ;
#18198 = EDGE_CURVE ( 'NONE', #5911, #2030, #19046, .T. ) ;
#18199 = EDGE_CURVE ( 'NONE', #1295, #14232, #9298, .T. ) ;
#18200 = EDGE_CURVE ( 'NONE', #1715, #13378, #7644, .T. ) ;
#18201 = CARTESIAN_POINT ( 'NONE',  ( 12.54492807148089284, -6.210945379539458244, -16.05864477962155590 ) ) ;
#18202 = EDGE_LOOP ( 'NONE', ( #21287, #16557, #4055, #12617 ) ) ;
#18203 = CARTESIAN_POINT ( 'NONE',  ( 9.271855056728114164, 14.88009260821627500, 7.115526499326136900 ) ) ;
#18204 = CARTESIAN_POINT ( 'NONE',  ( 38.31336037684268092, 38.28835795706343958, -4.744980486405671272 ) ) ;
#18205 = CARTESIAN_POINT ( 'NONE',  ( 9.765588637266073846, 21.83972979323944230, 3.602945500523575095 ) ) ;
#18206 = AXIS2_PLACEMENT_3D ( 'NONE', #11909, #16990, #1523 ) ;
#18207 = CARTESIAN_POINT ( 'NONE',  ( 19.92484631573285370, -4.252746759165957791, -15.32038969226572256 ) ) ;
#18208 = LINE ( 'NONE', #18300, #6366 ) ;
#18209 = ORIENTED_EDGE ( 'NONE', *, *, #15387, .T. ) ;
#18210 = CARTESIAN_POINT ( 'NONE',  ( 11.44401274691345094, 13.68327412096624229, 7.073018589382568777 ) ) ;
#18211 = DIRECTION ( 'NONE',  ( -0.000000000000000000, -1.000000000000000000, 0.000000000000000000 ) ) ;
#18212 = ORIENTED_EDGE ( 'NONE', *, *, #1837, .T. ) ;
#18213 = ORIENTED_EDGE ( 'NONE', *, *, #10493, .F. ) ;
#18214 = CARTESIAN_POINT ( 'NONE',  ( 8.505511374756364873, 39.28205249999999893, -20.97439202360551747 ) ) ;
#18215 = CARTESIAN_POINT ( 'NONE',  ( 2.189264113347045626, 19.81445010932126038, 0.4794500746898018306 ) ) ;
#18216 = VERTEX_POINT ( 'NONE', #18146 ) ;
#18217 = CARTESIAN_POINT ( 'NONE',  ( 5.557121319643879787, 21.53978237414855812, 3.555717224815803768 ) ) ;
#18218 = ORIENTED_EDGE ( 'NONE', *, *, #16726, .T. ) ;
#18219 = ORIENTED_EDGE ( 'NONE', *, *, #13554, .F. ) ;
#18220 = ADVANCED_FACE ( 'NONE', ( #14305 ), #21442, .T. ) ;
#18221 = DIRECTION ( 'NONE',  ( -0.7532174416907910786, 0.000000000000000000, -0.6577716059034319773 ) ) ;
#18222 = ORIENTED_EDGE ( 'NONE', *, *, #9944, .T. ) ;
#18223 = CARTESIAN_POINT ( 'NONE',  ( 4.587395795194475490, 11.87708295117914581, 3.824518294629957627 ) ) ;
#18224 = DIRECTION ( 'NONE',  ( -0.2672484743474505819, 0.000000000000000000, -0.9636276526537416176 ) ) ;
#18225 = LINE ( 'NONE', #3082, #4402 ) ;
#18226 = FACE_OUTER_BOUND ( 'NONE', #4870, .T. ) ;
#18227 = CARTESIAN_POINT ( 'NONE',  ( 1.951509951783207519, 18.39930244975314722, -0.2931944764921431412 ) ) ;
#18228 = ORIENTED_EDGE ( 'NONE', *, *, #17072, .F. ) ;
#18229 = CARTESIAN_POINT ( 'NONE',  ( 2.063750000000000195, 30.56076406250000232, 10.71562496029980061 ) ) ;
#18230 = CARTESIAN_POINT ( 'NONE',  ( 43.47225467835599488, 38.88803500000000213, -9.606390615344288619 ) ) ;
#18231 = DIRECTION ( 'NONE',  ( 0.000000000000000000, 1.000000000000000000, 0.000000000000000000 ) ) ;
#18232 = DIRECTION ( 'NONE',  ( -0.08420877549337302259, 0.000000000000000000, -0.9964481331860212121 ) ) ;
#18233 = ORIENTED_EDGE ( 'NONE', *, *, #9091, .T. ) ;
#18234 = ORIENTED_EDGE ( 'NONE', *, *, #6183, .T. ) ;
#18235 = CARTESIAN_POINT ( 'NONE',  ( 9.347881490430607343, 18.95229069147438139, -2.296150461628721384 ) ) ;
#18236 = DIRECTION ( 'NONE',  ( 0.000000000000000000, 1.000000000000000000, 0.000000000000000000 ) ) ;
#18237 = EDGE_LOOP ( 'NONE', ( #7498, #10131, #17575, #3069 ) ) ;
#18238 = ORIENTED_EDGE ( 'NONE', *, *, #18993, .F. ) ;
#18239 = DIRECTION ( 'NONE',  ( 0.000000000000000000, -1.000000000000000000, -0.000000000000000000 ) ) ;
#18240 = CARTESIAN_POINT ( 'NONE',  ( 9.271140109599555146, 14.96309120728511211, 7.029251134958126812 ) ) ;
#18241 = EDGE_CURVE ( 'NONE', #18464, #12469, #9620, .T. ) ;
#18242 = CARTESIAN_POINT ( 'NONE',  ( 59.61686353177688602, -3.968114999999999615, -0.7993558564620834028 ) ) ;
#18243 = CARTESIAN_POINT ( 'NONE',  ( 5.840875039352013687, 11.58534598419692152, 0.6053728465774781409 ) ) ;
#18244 = CARTESIAN_POINT ( 'NONE',  ( 0.1136883046600123126, 18.41686720684693412, 0.4625772567203307872 ) ) ;
#18245 = AXIS2_PLACEMENT_3D ( 'NONE', #4098, #2437, #17585 ) ;
#18246 = ORIENTED_EDGE ( 'NONE', *, *, #15074, .T. ) ;
#18247 = CARTESIAN_POINT ( 'NONE',  ( 0.2878105301525723525, 13.13938098413696132, 2.151847065340643628 ) ) ;
#18248 = DIRECTION ( 'NONE',  ( 0.000000000000000000, 1.000000000000000000, 0.000000000000000000 ) ) ;
#18249 = CARTESIAN_POINT ( 'NONE',  ( -1.427050033073577806, 26.98019749999999917, -23.44038945102687066 ) ) ;
#18250 = CARTESIAN_POINT ( 'NONE',  ( 13.13857632649210672, -7.757696357571966850, -15.48432750494124832 ) ) ;
#18251 = DIRECTION ( 'NONE',  ( -0.2868778675745011220, 0.000000000000000000, -0.9579671649362034858 ) ) ;
#18252 = EDGE_LOOP ( 'NONE', ( #7612, #1122, #8448, #2129 ) ) ;
#18253 = CARTESIAN_POINT ( 'NONE',  ( 10.86894147956441437, 19.58043239906450239, 6.762403744219564139 ) ) ;
#18254 = DIRECTION ( 'NONE',  ( 0.000000000000000000, 1.000000000000000000, 0.000000000000000000 ) ) ;
#18255 = CARTESIAN_POINT ( 'NONE',  ( 10.60219209945084273, 21.74929657561690277, 0.03335953411089977172 ) ) ;
#18256 = ORIENTED_EDGE ( 'NONE', *, *, #18024, .F. ) ;
#18257 = CARTESIAN_POINT ( 'NONE',  ( 9.078296277872521358, 19.06912958161391103, 7.286269445716254900 ) ) ;
#18258 = LINE ( 'NONE', #14755, #5252 ) ;
#18259 = CARTESIAN_POINT ( 'NONE',  ( 5.164072674603092494, 17.31775664876643006, 8.045972464850111194 ) ) ;
#18260 = CARTESIAN_POINT ( 'NONE',  ( 31.06384331886062711, 30.50833916023545811, 1.146004012482531476 ) ) ;
#18261 = CARTESIAN_POINT ( 'NONE',  ( 6.707929841484892464, 19.34112545770926062, 6.521503817312878759 ) ) ;
#18262 = EDGE_CURVE ( 'NONE', #12509, #13188, #4543, .T. ) ;
#18263 = AXIS2_PLACEMENT_3D ( 'NONE', #10742, #784, #15840 ) ;
#18264 = EDGE_CURVE ( 'NONE', #17843, #20607, #8113, .T. ) ;
#18265 = CARTESIAN_POINT ( 'NONE',  ( 38.82016491058538321, 32.54502000000000095, -14.75770094105646812 ) ) ;
#18266 = VERTEX_POINT ( 'NONE', #1223 ) ;
#18267 = CARTESIAN_POINT ( 'NONE',  ( 11.28455321728826988, 19.34515354661070319, 6.288198492919301330 ) ) ;
#18268 = CARTESIAN_POINT ( 'NONE',  ( 38.32982792479189271, -5.610959413415746333, -4.721377477347955320 ) ) ;
#18269 = CARTESIAN_POINT ( 'NONE',  ( 3.766814826540537453, 14.72191889613304205, 9.034809729852785409 ) ) ;
#18270 = DIRECTION ( 'NONE',  ( 0.000000000000000000, 1.000000000000000000, 0.000000000000000000 ) ) ;
#18271 = DIRECTION ( 'NONE',  ( 0.000000000000000000, -1.000000000000000000, 0.000000000000000000 ) ) ;
#18272 = CARTESIAN_POINT ( 'NONE',  ( -3.929154139288399961, 9.924415000000001541, 0.9374890779182719625 ) ) ;
#18273 = CARTESIAN_POINT ( 'NONE',  ( 59.90456643211351917, 0.000000000000000000, -2.926035437812116946 ) ) ;
#18274 = DIRECTION ( 'NONE',  ( -0.000000000000000000, -1.000000000000000000, 0.000000000000000000 ) ) ;
#18275 = VERTEX_POINT ( 'NONE', #11075 ) ;
#18276 = LINE ( 'NONE', #13223, #12827 ) ;
#18277 = CARTESIAN_POINT ( 'NONE',  ( 10.87724638690646017, 12.23061227675764151, 4.718482727644354391 ) ) ;
#18278 = ADVANCED_FACE ( 'NONE', ( #12742 ), #6300, .T. ) ;
#18279 = CARTESIAN_POINT ( 'NONE',  ( 54.55586098912687731, 0.000000000000000000, -6.056925149195119040 ) ) ;
#18280 = ORIENTED_EDGE ( 'NONE', *, *, #19262, .T. ) ;
#18281 = CARTESIAN_POINT ( 'NONE',  ( 12.41893761992812628, 11.32628166863733021, 2.535021602169117649 ) ) ;
#18282 = CARTESIAN_POINT ( 'NONE',  ( 17.99520596118501814, -14.84248999999999974, -14.84645223781840073 ) ) ;
#18283 = CARTESIAN_POINT ( 'NONE',  ( 11.36675820428501282, -3.110504336422511340, -16.48186686805254908 ) ) ;
#18285 = CARTESIAN_POINT ( 'NONE',  ( 59.61686353177688602, -1.983739999999999393, -0.7993558564620834028 ) ) ;
#18284 = CARTESIAN_POINT ( 'NONE',  ( 0.09077472999913152596, 18.62527059298274068, 1.328760847605261919 ) ) ;
#18286 = VERTEX_POINT ( 'NONE', #2888 ) ;
#18287 = SHAPE_REPRESENTATION_RELATIONSHIP ( 'NONE' , 'NONE' ,  #11018, #14338 ) ;
#18288 = CARTESIAN_POINT ( 'NONE',  ( 50.99913033092320092, 0.000000000000000000, -7.029081061492260751 ) ) ;
#18289 = CARTESIAN_POINT ( 'NONE',  ( 3.970142618090055198, 17.91763227041811746, -0.4079429902366753513 ) ) ;
#18290 = EDGE_CURVE ( 'NONE', #3524, #18035, #5868, .T. ) ;
#18291 = ORIENTED_EDGE ( 'NONE', *, *, #13685, .T. ) ;
#18292 = ADVANCED_FACE ( 'NONE', ( #19675 ), #4220, .T. ) ;
#18293 = CARTESIAN_POINT ( 'NONE',  ( 20.07739328931695511, -1.153533769354293748, -14.79997852497580979 ) ) ;
#18294 = AXIS2_PLACEMENT_3D ( 'NONE', #20783, #15841, #19344 ) ;
#18295 = CARTESIAN_POINT ( 'NONE',  ( 14.34014943933268071, 1.694275420233978036, -16.63941580623522398 ) ) ;
#18296 = ORIENTED_EDGE ( 'NONE', *, *, #5793, .F. ) ;
#18297 = CARTESIAN_POINT ( 'NONE',  ( 29.19635173153840313, 30.56064500000000095, -6.218966092919240296 ) ) ;
#18298 = CARTESIAN_POINT ( 'NONE',  ( 11.47995025628694599, 10.98646219477360297, -1.324771271245920090 ) ) ;
#18299 = CARTESIAN_POINT ( 'NONE',  ( 14.59124287633469308, -6.988731851215915114, -16.37203253287690785 ) ) ;
#18300 = CARTESIAN_POINT ( 'NONE',  ( -0.8970842057359728061, 5.548947500000001476, -22.54358764576276286 ) ) ;
#18301 = VERTEX_POINT ( 'NONE', #4335 ) ;
#18302 = CARTESIAN_POINT ( 'NONE',  ( 9.004191089903370582, 20.99879615889430085, 1.466809581464092016 ) ) ;
#18303 = CARTESIAN_POINT ( 'NONE',  ( 10.00188843905044855, 20.90159167551892239, -1.688002078711951626 ) ) ;
#18304 = ADVANCED_FACE ( 'NONE', ( #7750 ), #21232, .T. ) ;
#18305 = DIRECTION ( 'NONE',  ( -0.9987059298363657467, 0.000000000000000000, -0.05085730733808409287 ) ) ;
#18306 = ORIENTED_EDGE ( 'NONE', *, *, #797, .T. ) ;
#18307 = ORIENTED_EDGE ( 'NONE', *, *, #12203, .F. ) ;
#18308 = ADVANCED_FACE ( 'NONE', ( #13801 ), #8067, .F. ) ;
#18309 = AXIS2_PLACEMENT_3D ( 'NONE', #18828, #5338, #12103 ) ;
#18310 = DIRECTION ( 'NONE',  ( -0.7776383362760926898, 0.000000000000000000, 0.6287118719681938916 ) ) ;
#18312 = CARTESIAN_POINT ( 'NONE',  ( -16.73439918454169018, 37.15413452960619622, -25.92417111164088084 ) ) ;
#18311 = CARTESIAN_POINT ( 'NONE',  ( 0.2815462692566809144, 11.62092872259188070, 3.183352938865285697 ) ) ;
#18313 = ORIENTED_EDGE ( 'NONE', *, *, #10267, .F. ) ;
#18314 = CARTESIAN_POINT ( 'NONE',  ( 4.621627147662794144, 20.85603566110601292, 1.020116771113178666 ) ) ;
#18315 = ORIENTED_EDGE ( 'NONE', *, *, #16726, .F. ) ;
#18316 = ORIENTED_EDGE ( 'NONE', *, *, #3132, .T. ) ;
#18317 = CIRCLE ( 'NONE', #12324, 3.968750000000000000 ) ;
#18318 = FACE_OUTER_BOUND ( 'NONE', #6748, .T. ) ;
#18319 = EDGE_LOOP ( 'NONE', ( #16528, #11167, #12023, #6243, #7979, #14257 ) ) ;
#18320 = CARTESIAN_POINT ( 'NONE',  ( 11.23687375378556474, 14.18796137044646777, -4.074440146305448707 ) ) ;
#18321 = VECTOR ( 'NONE', #7169, 1000.000000000000114 ) ;
#18322 = FACE_OUTER_BOUND ( 'NONE', #2057, .T. ) ;
#18323 = DIRECTION ( 'NONE',  ( -0.9579671649362032637, -0.000000000000000000, 0.2868778675745010664 ) ) ;
#18324 = DIRECTION ( 'NONE',  ( -0.6702301885068628895, 0.000000000000000000, -0.7421532822901579785 ) ) ;
#18325 = CARTESIAN_POINT ( 'NONE',  ( 1.928551063676404942, 12.48261359942508264, 1.042194909420577131 ) ) ;
#18326 = ORIENTED_EDGE ( 'NONE', *, *, #19101, .T. ) ;
#18327 = DIRECTION ( 'NONE',  ( 0.000000000000000000, 1.000000000000000000, 0.000000000000000000 ) ) ;
#18328 = DIRECTION ( 'NONE',  ( -1.000000000000000000, 0.000000000000000000, 0.000000000000000000 ) ) ;
#18329 = DIRECTION ( 'NONE',  ( 1.000000000000000000, 0.000000000000000000, 0.000000000000000000 ) ) ;
#18330 = ADVANCED_FACE ( 'NONE', ( #15247 ), #21558, .T. ) ;
#18331 = CARTESIAN_POINT ( 'NONE',  ( 8.505511374756364873, -1.985327499999998357, -20.97439202360551747 ) ) ;
#18332 = ORIENTED_EDGE ( 'NONE', *, *, #16520, .T. ) ;
#18333 = EDGE_CURVE ( 'NONE', #10995, #20322, #185, .T. ) ;
#18334 = ORIENTED_EDGE ( 'NONE', *, *, #9671, .T. ) ;
#18335 = CARTESIAN_POINT ( 'NONE',  ( 8.841065195333532856, 12.18989644830414321, 5.119707677163611415 ) ) ;
#18336 = LINE ( 'NONE', #6402, #16845 ) ;
#18337 = ORIENTED_EDGE ( 'NONE', *, *, #3026, .F. ) ;
#18338 = ORIENTED_EDGE ( 'NONE', *, *, #13318, .F. ) ;
#18339 = CYLINDRICAL_SURFACE ( 'NONE', #1087, 3.968750000000000000 ) ;
#18340 = ORIENTED_EDGE ( 'NONE', *, *, #21504, .T. ) ;
#18341 = CARTESIAN_POINT ( 'NONE',  ( 8.925307470792780862, 12.29983341362659566, 5.083992750741611388 ) ) ;
#18342 = CARTESIAN_POINT ( 'NONE',  ( 6.493485979265003039, 11.70317488892350077, 3.279535273129327244 ) ) ;
#18343 = CARTESIAN_POINT ( 'NONE',  ( 53.69636427252483202, 38.88803500000000213, -18.48840734645144224 ) ) ;
#18344 = CARTESIAN_POINT ( 'NONE',  ( 3.768677667698563383, 12.20035416735056266, 0.3928182328957318670 ) ) ;
#18345 = CARTESIAN_POINT ( 'NONE',  ( -0.1933157125360287776, 15.43497882239525509, 0.1253114254156900143 ) ) ;
#18346 = CARTESIAN_POINT ( 'NONE',  ( 53.00421038040393995, -1.983739999999999837, 6.511420152579801446 ) ) ;
#18347 = AXIS2_PLACEMENT_3D ( 'NONE', #9557, #16434, #13118 ) ;
#18348 = ORIENTED_EDGE ( 'NONE', *, *, #7224, .F. ) ;
#18349 = APPLICATION_CONTEXT ( 'automotive_design' ) ;
#18350 = CARTESIAN_POINT ( 'NONE',  ( 6.278604723040791313, 20.44074137114568046, 5.191791585791021291 ) ) ;
#18351 = DIRECTION ( 'NONE',  ( 0.8334497143791951279, 0.000000000000000000, 0.5525953072558960066 ) ) ;
#18352 = LINE ( 'NONE', #2895, #15973 ) ;
#18353 = FACE_OUTER_BOUND ( 'NONE', #21194, .T. ) ;
#18354 = ORIENTED_EDGE ( 'NONE', *, *, #4095, .T. ) ;
#18355 = EDGE_CURVE ( 'NONE', #19859, #4163, #13692, .T. ) ;
#18356 = CARTESIAN_POINT ( 'NONE',  ( 8.539960005814746680, 10.73926345162572105, 3.719695862443936463 ) ) ;
#18357 = LINE ( 'NONE', #20225, #20871 ) ;
#18358 = CARTESIAN_POINT ( 'NONE',  ( 10.22900826487382808, 21.26279264426276328, -0.9859047892954733161 ) ) ;
#18359 = ORIENTED_EDGE ( 'NONE', *, *, #3420, .T. ) ;
#18360 = COLOUR_RGB ( '', 0.08235294, 0.09019608, 0.10196078) ;
#18361 = CARTESIAN_POINT ( 'NONE',  ( 6.290834976258575573, 20.61203802677264108, -0.1778393911984611497 ) ) ;
#18362 = DIRECTION ( 'NONE',  ( 0.000000000000000000, -1.000000000000000000, -0.000000000000000000 ) ) ;
#18363 = CARTESIAN_POINT ( 'NONE',  ( 46.03750000000000142, 0.000000000000000000, -10.31874999999999964 ) ) ;
#18364 = DIRECTION ( 'NONE',  ( 0.9579671649362033747, 0.000000000000000000, -0.2868778675745006779 ) ) ;
#18365 = AXIS2_PLACEMENT_3D ( 'NONE', #8519, #9845, #15299 ) ;
#18366 = DIRECTION ( 'NONE',  ( 0.000000000000000000, -1.000000000000000000, -0.000000000000000000 ) ) ;
#18367 = DIRECTION ( 'NONE',  ( 0.000000000000000000, 1.000000000000000000, 0.000000000000000000 ) ) ;
#18368 = CARTESIAN_POINT ( 'NONE',  ( 7.894657137420193038, 12.88806360044558197, -1.480813047728780640 ) ) ;
#18369 = CARTESIAN_POINT ( 'NONE',  ( 5.355787749307895140, 14.39168280676499556, 7.605419266839439807 ) ) ;
#18370 = CARTESIAN_POINT ( 'NONE',  ( 12.13621795668766445, -1.983739999999999393, 4.225309685850866082 ) ) ;
#18371 = CARTESIAN_POINT ( 'NONE',  ( 0.8536167157666036953, 11.31186333555498180, 4.830306691737135338 ) ) ;
#18372 = LINE ( 'NONE', #6981, #99 ) ;
#18373 = DIRECTION ( 'NONE',  ( 0.000000000000000000, -1.000000000000000000, -0.000000000000000000 ) ) ;
#18374 = DIRECTION ( 'NONE',  ( 0.08420877549337300871, 0.000000000000000000, 0.9964481331860212121 ) ) ;
#18375 = CARTESIAN_POINT ( 'NONE',  ( -13.57684171658811501, 32.54247999999999763, -0.8078590638549647540 ) ) ;
#18376 = CARTESIAN_POINT ( 'NONE',  ( 13.04853822875846348, -7.504789825882131282, -16.72033722309888759 ) ) ;
#18377 = AXIS2_PLACEMENT_3D ( 'NONE', #6515, #12948, #16475 ) ;
#18378 = PLANE ( 'NONE',  #1079 ) ;
#18379 = EDGE_CURVE ( 'NONE', #4031, #19334, #18618, .T. ) ;
#18380 = AXIS2_PLACEMENT_3D ( 'NONE', #14623, #21332, #12959 ) ;
#18381 = VERTEX_POINT ( 'NONE', #3621 ) ;
#18382 = CARTESIAN_POINT ( 'NONE',  ( 59.65121809612895731, 0.000000000000000000, -2.485718937265306572 ) ) ;
#18383 = ORIENTED_EDGE ( 'NONE', *, *, #4771, .F. ) ;
#18384 = CARTESIAN_POINT ( 'NONE',  ( 12.78616414870638351, 12.03792853171452215, 4.155831503912295055 ) ) ;
#18385 = DIRECTION ( 'NONE',  ( -0.2490110332224850509, 0.000000000000000000, 0.9685006480810792739 ) ) ;
#18386 = DIRECTION ( 'NONE',  ( 0.2490110332224855227, 0.000000000000000000, -0.9685006480810791629 ) ) ;
#18387 = CARTESIAN_POINT ( 'NONE',  ( 17.16396544380940270, -7.327104899143136230, -15.69103126553038408 ) ) ;
#18388 = CYLINDRICAL_SURFACE ( 'NONE', #17708, 1.983740000000000281 ) ;
#18389 = VERTEX_POINT ( 'NONE', #8471 ) ;
#18390 = SHAPE_REPRESENTATION_RELATIONSHIP ( 'NONE' , 'NONE' ,  #21464, #9295 ) ;
#18391 = CARTESIAN_POINT ( 'NONE',  ( 2.915917464538113180, 34.52875999999999834, -18.72348548116188027 ) ) ;
#18392 = ORIENTED_EDGE ( 'NONE', *, *, #20646, .T. ) ;
#18393 = CARTESIAN_POINT ( 'NONE',  ( 6.176127164391592927, 10.98645767192390110, 2.860351699068144349 ) ) ;
#18394 = AXIS2_PLACEMENT_3D ( 'NONE', #16951, #20039, #13547 ) ;
#18395 = AXIS2_PLACEMENT_3D ( 'NONE', #6258, #9787, #21509 ) ;
#18396 = CARTESIAN_POINT ( 'NONE',  ( 14.91906957739207762, -7.556863888178527944, -15.56863359939283242 ) ) ;
#18397 = ORIENTED_EDGE ( 'NONE', *, *, #7381, .F. ) ;
#18398 = CARTESIAN_POINT ( 'NONE',  ( 8.914303899894372663, 12.18626401121546188, 5.100153663711656016 ) ) ;
#18399 = ADVANCED_FACE ( 'NONE', ( #15469 ), #3505, .T. ) ;
#18400 = CARTESIAN_POINT ( 'NONE',  ( 38.49896492022744354, 37.93513121111498521, -4.495645369696349647 ) ) ;
#18401 = CARTESIAN_POINT ( 'NONE',  ( 7.176325731368327965, 14.38111527192631200, -2.643793538748910876 ) ) ;
#18402 = AXIS2_PLACEMENT_3D ( 'NONE', #14743, #6306, #4774 ) ;
#18403 = VECTOR ( 'NONE', #9632, 1000.000000000000000 ) ;
#18404 = CARTESIAN_POINT ( 'NONE',  ( 12.71419532639660588, -5.571168796945357826, -16.74134232755136864 ) ) ;
#18405 = CARTESIAN_POINT ( 'NONE',  ( 0.7843704457339527591, 25.39269750000000059, -23.55949434567611078 ) ) ;
#18406 = EDGE_CURVE ( 'NONE', #8918, #8259, #11294, .T. ) ;
#18407 = B_SPLINE_CURVE_WITH_KNOTS ( 'NONE', 3,
 ( #7980, #16085, #915, #4459, #17844, #11190, #21351, #4559, #10974, #19478, #21457, #1127, #11299, #7870, #6102, #2789, #18048, #1016, #6316, #5883, #4235, #7763, #12645, #21247, #17728, #2578, #14419, #21134, #5987, #12757, #4349, #14530, #646, #2081, #17463, #7291, #15716, #18992, #873, #12598, #13951, #757, #20649, #20872, #2307, #10822, #9043 ),
 .UNSPECIFIED., .F., .F.,
 ( 4, 1, 1, 1, 1, 1, 1, 1, 1, 1, 1, 1, 1, 1, 1, 1, 1, 1, 1, 1, 1, 1, 1, 1, 1, 1, 1, 1, 1, 1, 1, 1, 1, 1, 1, 1, 1, 1, 1, 1, 1, 1, 1, 1, 4 ),
 ( 0.000000000000000000, 0.02272727272726999745, 0.04545454545455000078, 0.06818181818181999476, 0.09090909090909000956, 0.1136363636363999924, 0.1363636363635999937, 0.1590909090909000123, 0.1818181818182000031, 0.2045454545454999939, 0.2272727272727000092, 0.2500000000000000000, 0.2727272727273000186, 0.2954545454545000061, 0.3181818181818000246, 0.3409090909091000432, 0.3636363636364000063, 0.3863636363635999937, 0.4090909090909000123, 0.4318181818182000309, 0.4545454545454999939, 0.4772727272726999814, 0.5000000000000000000, 0.5227272727273000186, 0.5454545454545000061, 0.5681818181818000246, 0.5909090909091000432, 0.6136363636364000618, 0.6363636363636000493, 0.6590909090908999568, 0.6818181818181999754, 0.7045454545454999939, 0.7272727272726999814, 0.7500000000000000000, 0.7727272727273000186, 0.7954545454545000061, 0.8181818181818000246, 0.8409090909091000432, 0.8636363636364000618, 0.8863636363636000493, 0.9090909090908999568, 0.9318181818181999754, 0.9545454545454999939, 0.9772727272726999814, 1.000000000000000000 ),
 .UNSPECIFIED. ) ;
#18408 = ORIENTED_EDGE ( 'NONE', *, *, #11699, .F. ) ;
#18409 = EDGE_CURVE ( 'NONE', #15141, #9888, #12243, .T. ) ;
#18410 = EDGE_CURVE ( 'NONE', #12574, #4315, #14146, .T. ) ;
#18411 = CARTESIAN_POINT ( 'NONE',  ( 9.496038166692052584, 21.06521520967978134, 2.786730198130631386 ) ) ;
#18412 = CARTESIAN_POINT ( 'NONE',  ( 9.501456576801587062, 16.63233464712778087, 8.082444101715321239 ) ) ;
#18413 = DIRECTION ( 'NONE',  ( -0.08420877549337300871, 0.000000000000000000, -0.9964481331860212121 ) ) ;
#18414 = ORIENTED_EDGE ( 'NONE', *, *, #18262, .F. ) ;
#18415 = ORIENTED_EDGE ( 'NONE', *, *, #6140, .F. ) ;
#18416 = AXIS2_PLACEMENT_3D ( 'NONE', #19901, #12973, #7863 ) ;
#18417 = AXIS2_PLACEMENT_3D ( 'NONE', #1099, #9607, #10941 ) ;
#18418 = FACE_OUTER_BOUND ( 'NONE', #9879, .T. ) ;
#18420 = DIRECTION ( 'NONE',  ( 0.000000000000000000, 1.000000000000000000, 0.000000000000000000 ) ) ;
#18419 = CARTESIAN_POINT ( 'NONE',  ( -0.4161015405540489098, 21.11857065418899992, 4.799063142585588082 ) ) ;
#18421 = EDGE_LOOP ( 'NONE', ( #4568, #4638, #14477 ) ) ;
#18422 = CARTESIAN_POINT ( 'NONE',  ( 6.488669288154311765, 20.75080086149703718, 6.076603587721198352 ) ) ;
#18423 = ORIENTED_EDGE ( 'NONE', *, *, #6557, .F. ) ;
#18424 = VECTOR ( 'NONE', #8800, 1000.000000000000114 ) ;
#18425 = EDGE_LOOP ( 'NONE', ( #6488, #3852, #19447, #21329 ) ) ;
#18426 = VECTOR ( 'NONE', #13728, 1000.000000000000227 ) ;
#18427 = DIRECTION ( 'NONE',  ( 0.000000000000000000, 1.000000000000000000, 0.000000000000000000 ) ) ;
#18428 = VERTEX_POINT ( 'NONE', #8688 ) ;
#18429 = EDGE_CURVE ( 'NONE', #15950, #7495, #5485, .T. ) ;
#18430 = TOROIDAL_SURFACE ( 'NONE', #11735, 3.174999999999999822, 1.190625000000000044 ) ;
#18431 = CARTESIAN_POINT ( 'NONE',  ( 9.461694371501065959, 12.85627548497952155, 6.928812902285866215 ) ) ;
#18432 = CIRCLE ( 'NONE', #14583, 30.16249999999998366 ) ;
#18433 = LINE ( 'NONE', #1623, #18786 ) ;
#18434 = CARTESIAN_POINT ( 'NONE',  ( 13.67756757867809725, 38.48766750000000059, 2.571257636385987144 ) ) ;
#18435 = CARTESIAN_POINT ( 'NONE',  ( 1.811815405336057783, 13.09036154768227611, 0.4682391260633863572 ) ) ;
#18436 = CIRCLE ( 'NONE', #19151, 0.5953125000000005773 ) ;
#18437 = AXIS2_PLACEMENT_3D ( 'NONE', #5712, #9349, #7482 ) ;
#18438 = VERTEX_POINT ( 'NONE', #292 ) ;
#18439 = ADVANCED_FACE ( 'NONE', ( #5059, #8793 ), #16989, .T. ) ;
#18440 = DIRECTION ( 'NONE',  ( 0.000000000000000000, 1.000000000000000000, 0.000000000000000000 ) ) ;
#18441 = FACE_OUTER_BOUND ( 'NONE', #21872, .T. ) ;
#18442 = CARTESIAN_POINT ( 'NONE',  ( 23.00195419928544638, 28.96330250000000461, -15.19829965147284945 ) ) ;
#18443 = VERTEX_POINT ( 'NONE', #6715 ) ;
#18444 = ORIENTED_EDGE ( 'NONE', *, *, #4372, .F. ) ;
#18445 = CARTESIAN_POINT ( 'NONE',  ( 9.026333315608731311, 21.14801334772412034, 1.793015295882868898 ) ) ;
#18446 = B_SPLINE_CURVE_WITH_KNOTS ( 'NONE', 3,
 ( #18912, #20561, #10517, #15960, #12189 ),
 .UNSPECIFIED., .F., .F.,
 ( 4, 1, 4 ),
 ( 0.000000000000000000, 2.695145555969153257E-05, 5.390291111938306514E-05 ),
 .UNSPECIFIED. ) ;
#18447 = ORIENTED_EDGE ( 'NONE', *, *, #14435, .F. ) ;
#18448 = AXIS2_PLACEMENT_3D ( 'NONE', #20845, #20622, #2402 ) ;
#18449 = VERTEX_POINT ( 'NONE', #3841 ) ;
#18450 = CARTESIAN_POINT ( 'NONE',  ( 21.03437500000000071, 0.000000000000000000, 5.159374999999999822 ) ) ;
#18451 = VERTEX_POINT ( 'NONE', #18540 ) ;
#18452 = CARTESIAN_POINT ( 'NONE',  ( 8.687903267574414556, 11.77246275954110644, 4.005785389838548483 ) ) ;
#18453 = AXIS2_PLACEMENT_3D ( 'NONE', #13493, #10157, #8609 ) ;
#18454 = AXIS2_PLACEMENT_3D ( 'NONE', #16931, #13317, #15088 ) ;
#18455 = CARTESIAN_POINT ( 'NONE',  ( 3.271205700320040322, 17.33608809750036883, 8.332789245943363454 ) ) ;
#18456 = EDGE_CURVE ( 'NONE', #11378, #13886, #20392, .T. ) ;
#18457 = EDGE_CURVE ( 'NONE', #15003, #2583, #14854, .T. ) ;
#18458 = EDGE_CURVE ( 'NONE', #8237, #16767, #5376, .T. ) ;
#18459 = DIRECTION ( 'NONE',  ( 0.4564177847958862944, -0.8819931412481734068, 0.1173494972856528179 ) ) ;
#18460 = AXIS2_PLACEMENT_3D ( 'NONE', #15041, #18642, #5162 ) ;
#18461 = CARTESIAN_POINT ( 'NONE',  ( 41.78116128337411794, 32.54502000000000095, 7.392073290253172502 ) ) ;
#18462 = DIRECTION ( 'NONE',  ( 0.000000000000000000, 1.000000000000000000, 0.000000000000000000 ) ) ;
#18463 = CARTESIAN_POINT ( 'NONE',  ( -0.1373303213323190108, 13.91591237273533643, 0.6777295261262165083 ) ) ;
#18464 = VERTEX_POINT ( 'NONE', #10467 ) ;
#18465 = CARTESIAN_POINT ( 'NONE',  ( 5.483205516165491566, 15.73838188847654784, 8.059224173191235963 ) ) ;
#18466 = FACE_OUTER_BOUND ( 'NONE', #747, .T. ) ;
#18467 = CARTESIAN_POINT ( 'NONE',  ( 52.59520707473905787, -7.308466495983068967, -17.22774659103923156 ) ) ;
#18468 = CARTESIAN_POINT ( 'NONE',  ( 50.99913033092320092, 32.54502000000000095, -7.029081061492260751 ) ) ;
#18469 = CARTESIAN_POINT ( 'NONE',  ( 29.01020070778135818, 36.51313500000000545, -13.85841188422236492 ) ) ;
#18470 = VERTEX_POINT ( 'NONE', #15572 ) ;
#18471 = CARTESIAN_POINT ( 'NONE',  ( 5.181714843770189205, 17.39297272447799614, -2.004891181105121767 ) ) ;
#18472 = CIRCLE ( 'NONE', #19227, 0.5080000000000002292 ) ;
#18473 = CARTESIAN_POINT ( 'NONE',  ( 13.16653485932300605, 18.18704292219559804, 6.886964970145631248 ) ) ;
#18474 = ORIENTED_EDGE ( 'NONE', *, *, #10660, .T. ) ;
#18475 = CARTESIAN_POINT ( 'NONE',  ( 6.795993791136487161, 21.39258517102323154, 1.175440690275210587 ) ) ;
#18476 = CARTESIAN_POINT ( 'NONE',  ( 50.99913033092320092, 0.000000000000000000, -7.029081061492260751 ) ) ;
#18477 = DIRECTION ( 'NONE',  ( 0.8583349619704310207, 0.000000000000000000, -0.5130897514657826175 ) ) ;
#18478 = CARTESIAN_POINT ( 'NONE',  ( 6.648854909583223893, 19.49398999500200702, 6.377479405198467788 ) ) ;
#18479 = CARTESIAN_POINT ( 'NONE',  ( -29.36874999999999858, 0.000000000000000000, 10.71562499999999929 ) ) ;
#18480 = EDGE_CURVE ( 'NONE', #4038, #9564, #12378, .T. ) ;
#18481 = LINE ( 'NONE', #238, #21866 ) ;
#18482 = AXIS2_PLACEMENT_3D ( 'NONE', #20387, #1941, #1725 ) ;
#18483 = CARTESIAN_POINT ( 'NONE',  ( 11.07157954474111250, 21.50410229886458424, 0.05352075458857742662 ) ) ;
#18484 = CARTESIAN_POINT ( 'NONE',  ( 7.224192598190189329, 11.65531656196440125, 5.982166327705092712 ) ) ;
#18485 = CARTESIAN_POINT ( 'NONE',  ( 27.87822510359947614, 32.54502000000000095, -8.893823290944665061 ) ) ;
#18486 = LINE ( 'NONE', #2927, #9610 ) ;
#18487 = FACE_OUTER_BOUND ( 'NONE', #2314, .T. ) ;
#18488 = DIRECTION ( 'NONE',  ( 0.9943660382494290406, 0.000000000000000000, -0.1060008583745199739 ) ) ;
#18489 = CARTESIAN_POINT ( 'NONE',  ( 0.02083138522551555155, 12.30439499999999953, 7.210477125664100484 ) ) ;
#18490 = CARTESIAN_POINT ( 'NONE',  ( 13.81931296094454531, -7.948541684644407468, -16.55524147760729647 ) ) ;
#18491 = CARTESIAN_POINT ( 'NONE',  ( -6.268352501591477832, -0.7997824999999986195, -35.49402737582407497 ) ) ;
#18492 = ORIENTED_EDGE ( 'NONE', *, *, #8938, .F. ) ;
#18493 = CARTESIAN_POINT ( 'NONE',  ( 46.03750000000000142, 0.000000000000000000, -10.31874999999999964 ) ) ;
#18494 = CARTESIAN_POINT ( 'NONE',  ( 11.56192577415882816, -1.983739999999999393, 4.677561850332325299 ) ) ;
#18495 = CARTESIAN_POINT ( 'NONE',  ( 12.61159337879046838, 19.40172461140289073, 5.406710191991988879 ) ) ;
#18496 = CARTESIAN_POINT ( 'NONE',  ( 17.40805163412996492, -7.126251874856905921, -14.42423430082585156 ) ) ;
#18498 = DIRECTION ( 'NONE',  ( 0.000000000000000000, -1.000000000000000000, -0.000000000000000000 ) ) ;
#18497 = CARTESIAN_POINT ( 'NONE',  ( 4.982102255498003451, 17.33943586079730181, 8.193447612696807880 ) ) ;
#18499 = VECTOR ( 'NONE', #15747, 1000.000000000000227 ) ;
#18500 = EDGE_LOOP ( 'NONE', ( #8340, #14286 ) ) ;
#18501 = CARTESIAN_POINT ( 'NONE',  ( 0.000000000000000000, 0.000000000000000000, 0.000000000000000000 ) ) ;
#18502 = CARTESIAN_POINT ( 'NONE',  ( -0.4828751281428080300, 20.94457815382166288, 5.240160791693938336 ) ) ;
#18503 = CARTESIAN_POINT ( 'NONE',  ( 3.766650751444651224, 16.23556631072887768, -0.6615111522120750154 ) ) ;
#18504 = DIRECTION ( 'NONE',  ( -0.6702301885068639997, 0.000000000000000000, -0.7421532822901570903 ) ) ;
#18505 = CARTESIAN_POINT ( 'NONE',  ( 6.030241924700674438, 11.44921767649160138, 2.937825647248552663 ) ) ;
#18506 = AXIS2_PLACEMENT_3D ( 'NONE', #13668, #20370, #5234 ) ;
#18507 = EDGE_CURVE ( 'NONE', #1126, #19175, #10424, .T. ) ;
#18508 = CARTESIAN_POINT ( 'NONE',  ( 20.53300515663952908, -0.2355993312742575563, -15.47241927149025109 ) ) ;
#18509 = ORIENTED_EDGE ( 'NONE', *, *, #2816, .F. ) ;
#18510 = CARTESIAN_POINT ( 'NONE',  ( 7.635144067882908558, 18.07295993736750361, -1.933075387652198440 ) ) ;
#18511 = CARTESIAN_POINT ( 'NONE',  ( 3.857526900225019428, 20.53171221136609503, 4.646854770459164286 ) ) ;
#18512 = CARTESIAN_POINT ( 'NONE',  ( 10.32152984533092521, 11.26381867368412060, 2.173457052760668251 ) ) ;
#18513 = DIRECTION ( 'NONE',  ( -1.000000000000000000, 0.000000000000000000, 0.000000000000000000 ) ) ;
#18514 = CARTESIAN_POINT ( 'NONE',  ( 9.120059585750226461, 17.37232422777100993, -3.649286426821030993 ) ) ;
#18515 = CIRCLE ( 'NONE', #5106, 0.7950200000000000600 ) ;
#18516 = EDGE_CURVE ( 'NONE', #9986, #13702, #6364, .T. ) ;
#18517 = CARTESIAN_POINT ( 'NONE',  ( 11.91164091833190852, -3.559739266059170681, -16.84475823795191829 ) ) ;
#18518 = CARTESIAN_POINT ( 'NONE',  ( 53.00421038040393995, 34.52875999999999834, 6.511420152579801446 ) ) ;
#18519 = ORIENTED_EDGE ( 'NONE', *, *, #14653, .F. ) ;
#18520 = CARTESIAN_POINT ( 'NONE',  ( 10.28124151015280852, 20.25644008567019583, 4.865497118489055417 ) ) ;
#18521 = CARTESIAN_POINT ( 'NONE',  ( 11.15139589856166147, 12.31865010030356089, -2.978430479911657436 ) ) ;
#18522 = CARTESIAN_POINT ( 'NONE',  ( 23.41562500000000213, 1.984375000000000000, 5.159374999999999822 ) ) ;
#18523 = CIRCLE ( 'NONE', #20991, 30.16249999999999787 ) ;
#18524 = ORIENTED_EDGE ( 'NONE', *, *, #2764, .F. ) ;
#18525 = ORIENTED_EDGE ( 'NONE', *, *, #6926, .T. ) ;
#18526 = CARTESIAN_POINT ( 'NONE',  ( 53.13666646117270886, -5.167180607494337607, -16.66914697179084826 ) ) ;
#18527 = CARTESIAN_POINT ( 'NONE',  ( 11.15439167821005029, 12.38857047172271031, -2.867789696427907931 ) ) ;
#18529 = CARTESIAN_POINT ( 'NONE',  ( 1.670997140563193373, -1.594802499999999013, -22.76294857149378714 ) ) ;
#18528 = CARTESIAN_POINT ( 'NONE',  ( 2.172710587819679517, 11.29961739780916119, 3.546512833330152326 ) ) ;
#18530 = ORIENTED_EDGE ( 'NONE', *, *, #1883, .F. ) ;
#18531 = CARTESIAN_POINT ( 'NONE',  ( 5.516160446314412269, 21.53913100960356175, 3.443779750929269579 ) ) ;
#18532 = ORIENTED_EDGE ( 'NONE', *, *, #5374, .T. ) ;
#18533 = EDGE_CURVE ( 'NONE', #16034, #19608, #2117, .T. ) ;
#18534 = LINE ( 'NONE', #3399, #17322 ) ;
#18535 = ORIENTED_EDGE ( 'NONE', *, *, #3143, .T. ) ;
#18536 = ADVANCED_FACE ( 'NONE', ( #5212 ), #5003, .T. ) ;
#18537 = CIRCLE ( 'NONE', #9006, 0.5079999999999984528 ) ;
#18538 = CARTESIAN_POINT ( 'NONE',  ( 3.748624155036380579, 14.56599487236573687, -0.2957577876794132421 ) ) ;
#18539 = CARTESIAN_POINT ( 'NONE',  ( 26.59062499999999929, 1.984375000000000000, 8.335010000000000474 ) ) ;
#18540 = CARTESIAN_POINT ( 'NONE',  ( 2.417820406479087580, 33.48813496001219647, -22.53959718991430350 ) ) ;
#18541 = DIRECTION ( 'NONE',  ( 0.000000000000000000, 1.000000000000000000, 0.000000000000000000 ) ) ;
#18542 = CARTESIAN_POINT ( 'NONE',  ( 1.672457707464642063, 14.56602435239780746, -0.3694984668618649382 ) ) ;
#18543 = ORIENTED_EDGE ( 'NONE', *, *, #11172, .F. ) ;
#18544 = CARTESIAN_POINT ( 'NONE',  ( 36.73521423675246922, 32.54502000000000095, 2.413462327205186497 ) ) ;
#18545 = FACE_OUTER_BOUND ( 'NONE', #19442, .T. ) ;
#18546 = LINE ( 'NONE', #5384, #7143 ) ;
#18547 = LINE ( 'NONE', #9416, #8168 ) ;
#18549 = CARTESIAN_POINT ( 'NONE',  ( 17.65755290411736311, -6.728872469205175122, -14.52017334799040782 ) ) ;
#18548 = CARTESIAN_POINT ( 'NONE',  ( -1.427050033073577806, 25.39269750000000059, -23.44038945102687066 ) ) ;
#18550 = EDGE_LOOP ( 'NONE', ( #21478, #17097, #13298, #16227 ) ) ;
#18551 = ORIENTED_EDGE ( 'NONE', *, *, #18805, .T. ) ;
#18552 = CARTESIAN_POINT ( 'NONE',  ( 8.921930343624811854, 18.23105645554593934, 6.967881739085774129 ) ) ;
#18553 = CARTESIAN_POINT ( 'NONE',  ( -0.8735635081908617039, 20.56277232864792026, 3.239896734077844176 ) ) ;
#18554 = ORIENTED_EDGE ( 'NONE', *, *, #4912, .T. ) ;
#18555 = EDGE_CURVE ( 'NONE', #18960, #17030, #17051, .T. ) ;
#18556 = CIRCLE ( 'NONE', #9022, 0.3962399999999998146 ) ;
#18557 = VERTEX_POINT ( 'NONE', #15419 ) ;
#18558 = CARTESIAN_POINT ( 'NONE',  ( -17.46249999999999858, 16.27314499999999953, 8.731249999999999289 ) ) ;
#18559 = ORIENTED_EDGE ( 'NONE', *, *, #9773, .F. ) ;
#18560 = CARTESIAN_POINT ( 'NONE',  ( 8.398975721931316585, 11.53959439960164168, 2.731685725725969238 ) ) ;
#18561 = EDGE_CURVE ( 'NONE', #11296, #19395, #13533, .T. ) ;
#18562 = EDGE_CURVE ( 'NONE', #4289, #2298, #11968, .T. ) ;
#18563 = CARTESIAN_POINT ( 'NONE',  ( -14.35397337327049172, 33.73373999999999739, -0.6462872510839714479 ) ) ;
#18564 = DIRECTION ( 'NONE',  ( -0.7421532822901579785, 0.000000000000000000, 0.6702301885068628895 ) ) ;
#18565 = CARTESIAN_POINT ( 'NONE',  ( -0.08781225755531263388, 13.44674506006041170, 0.9678096409466712124 ) ) ;
#18566 = DIRECTION ( 'NONE',  ( 0.9129422336036140395, 0.000000000000000000, -0.4080888115384250225 ) ) ;
#18567 = ORIENTED_EDGE ( 'NONE', *, *, #4769, .T. ) ;
#18568 = CARTESIAN_POINT ( 'NONE',  ( 7.337216344270507840, 13.47382733369860119, 6.754120465228507619 ) ) ;
#18569 = LINE ( 'NONE', #10064, #12428 ) ;
#18570 = CARTESIAN_POINT ( 'NONE',  ( 59.89111109153450485, -4.569743463999999200, -22.14529389979288965 ) ) ;
#18571 = CARTESIAN_POINT ( 'NONE',  ( 53.25483508941461963, -9.531985000000000596, -5.879799058943532941 ) ) ;
#18572 = DIRECTION ( 'NONE',  ( 0.000000000000000000, 1.000000000000000000, 0.000000000000000000 ) ) ;
#18573 = ORIENTED_EDGE ( 'NONE', *, *, #10758, .T. ) ;
#18574 = CARTESIAN_POINT ( 'NONE',  ( 9.479482390282207405, 21.75488213915048163, 3.666800339307922485 ) ) ;
#18575 = CARTESIAN_POINT ( 'NONE',  ( 12.93232447009971509, 19.36079900857183489, 6.353122240160271161 ) ) ;
#18576 = VERTEX_POINT ( 'NONE', #13754 ) ;
#18577 = ADVANCED_FACE ( 'NONE', ( #18812 ), #12637, .F. ) ;
#18578 = EDGE_CURVE ( 'NONE', #18301, #7937, #14088, .T. ) ;
#18579 = EDGE_CURVE ( 'NONE', #119, #13886, #7426, .T. ) ;
#18580 = CARTESIAN_POINT ( 'NONE',  ( 9.494406476674157602, 15.01763621828074236, 7.831721205212923032 ) ) ;
#18581 = CARTESIAN_POINT ( 'NONE',  ( 4.125927529995728094, 18.69411302701743338, -0.1543514116386320856 ) ) ;
#18582 = DIRECTION ( 'NONE',  ( 0.000000000000000000, 1.000000000000000000, 0.000000000000000000 ) ) ;
#18583 = CARTESIAN_POINT ( 'NONE',  ( 7.323328843850104519, 15.41683489813229180, 7.541440311446245381 ) ) ;
#18584 = DIRECTION ( 'NONE',  ( 0.9964481331860212121, 0.000000000000000000, -0.08420877549337300871 ) ) ;
#18585 = CARTESIAN_POINT ( 'NONE',  ( 13.16571366779050223, 21.56964499642510091, 0.3938296393673330065 ) ) ;
#18586 = CARTESIAN_POINT ( 'NONE',  ( 5.449727700892514015, 12.34694125381258267, 7.158361069179933089 ) ) ;
#18587 = CARTESIAN_POINT ( 'NONE',  ( 17.87574706213523612, 34.52875999999999834, -11.18912023382283571 ) ) ;
#18588 = CARTESIAN_POINT ( 'NONE',  ( 20.23691056526638832, -1.234862104235166402, -14.75547226453677219 ) ) ;
#18589 = LINE ( 'NONE', #20450, #3700 ) ;
#18590 = CARTESIAN_POINT ( 'NONE',  ( 201.9384738932629944, 2.380615000000000148, 8.335010000000000474 ) ) ;
#18591 = CARTESIAN_POINT ( 'NONE',  ( 10.72696675674987254, -2.863640533428135626, -17.11876806796568573 ) ) ;
#18592 = CARTESIAN_POINT ( 'NONE',  ( 17.22522857595987844, -3.968114999999999615, -15.04442098945225403 ) ) ;
#18593 = EDGE_LOOP ( 'NONE', ( #9732, #753, #9492, #17886 ) ) ;
#18594 = DIRECTION ( 'NONE',  ( -0.2490110332224850231, 0.000000000000000000, 0.9685006480810791629 ) ) ;
#18595 = CARTESIAN_POINT ( 'NONE',  ( 9.372025013462977228, 21.88221636350534993, 2.458001116284384668 ) ) ;
#18596 = CARTESIAN_POINT ( 'NONE',  ( 38.28489021960990613, 38.88803500000000213, 2.732679409805250703 ) ) ;
#18597 = EDGE_CURVE ( 'NONE', #8797, #2943, #720, .T. ) ;
#18598 = VERTEX_POINT ( 'NONE', #3902 ) ;
#18599 = EDGE_CURVE ( 'NONE', #13188, #10888, #21180, .T. ) ;
#18600 = CARTESIAN_POINT ( 'NONE',  ( 13.01173305175439232, 17.52789639782027109, 6.278958820054959311 ) ) ;
#18601 = AXIS2_PLACEMENT_3D ( 'NONE', #15799, #12919, #4396 ) ;
#18602 = CARTESIAN_POINT ( 'NONE',  ( 11.76433965462081055, -4.504481791847095629, -15.74942804055007706 ) ) ;
#18604 = DIRECTION ( 'NONE',  ( 1.000000000000000000, 0.000000000000000000, 0.000000000000000000 ) ) ;
#18603 = CARTESIAN_POINT ( 'NONE',  ( 5.095392006347933211, 14.17727879546418812, 7.782683345560178267 ) ) ;
#18605 = ORIENTED_EDGE ( 'NONE', *, *, #18507, .T. ) ;
#18606 = CARTESIAN_POINT ( 'NONE',  ( -0.8970842057359728061, 5.548947500000001476, -22.54358764576276286 ) ) ;
#18607 = CARTESIAN_POINT ( 'NONE',  ( 4.546228995060008771, 19.82055208975022254, 0.9194446738514544526 ) ) ;
#18608 = CYLINDRICAL_SURFACE ( 'NONE', #16223, 25.00312499999999361 ) ;
#18609 = CARTESIAN_POINT ( 'NONE',  ( 6.025094433076758627, 11.18924701328941040, 2.920388319698000501 ) ) ;
#18610 = CARTESIAN_POINT ( 'NONE',  ( 11.57003115466494769, 0.1030431252659232133, -17.27253179266325489 ) ) ;
#18611 = ORIENTED_EDGE ( 'NONE', *, *, #20772, .F. ) ;
#18612 = CARTESIAN_POINT ( 'NONE',  ( 13.11702139709938386, 16.70050942663215210, 6.509090343710545845 ) ) ;
#18613 = CARTESIAN_POINT ( 'NONE',  ( 7.580253574866159916, 13.14813038638666143, -1.062414283180728614 ) ) ;
#18614 = CARTESIAN_POINT ( 'NONE',  ( 2.786775659238538871, 19.53481664226216452, 0.6126602542314601996 ) ) ;
#18615 = CARTESIAN_POINT ( 'NONE',  ( 9.948484665932129545, 20.90159167551892239, -1.672009504943896552 ) ) ;
#18616 = CARTESIAN_POINT ( 'NONE',  ( 13.81552360302172922, -6.599745701269019271, -16.53000304243150964 ) ) ;
#18617 = DIRECTION ( 'NONE',  ( 0.000000000000000000, 1.000000000000000000, 0.000000000000000000 ) ) ;
#18618 =( BOUNDED_CURVE ( )  B_SPLINE_CURVE ( 3, ( #18864, #11810, #1730, #18967 ),
 .UNSPECIFIED., .F., .F. ) 
 B_SPLINE_CURVE_WITH_KNOTS ( ( 4, 4 ),
 ( 4.712388980384379700, 5.083959002914050451 ),
 .UNSPECIFIED. ) 
 CURVE ( )  GEOMETRIC_REPRESENTATION_ITEM ( )  RATIONAL_B_SPLINE_CURVE ( ( 1.000000000000000000, 0.9885276984536621736, 0.9885276984536621736, 1.000000000000000000 ) ) 
 REPRESENTATION_ITEM ( '' )  );
#18619 = ORIENTED_EDGE ( 'NONE', *, *, #10660, .F. ) ;
#18620 = CARTESIAN_POINT ( 'NONE',  ( 8.087630817559809060, 19.60821679331170486, -0.9184393018855864232 ) ) ;
#18621 = CARTESIAN_POINT ( 'NONE',  ( 12.86638604525510843, 22.28511555871962102, 0.3811982759095605133 ) ) ;
#18622 = ORIENTED_EDGE ( 'NONE', *, *, #20179, .F. ) ;
#18623 = VERTEX_POINT ( 'NONE', #2119 ) ;
#18624 = EDGE_CURVE ( 'NONE', #10134, #13027, #13099, .T. ) ;
#18625 = CARTESIAN_POINT ( 'NONE',  ( 49.13030338002142372, -1.983739999999999837, -2.154981381712871791 ) ) ;
#18626 = CARTESIAN_POINT ( 'NONE',  ( 10.99961054126760729, 17.04339191392503494, -4.321057179415156213 ) ) ;
#18628 = CARTESIAN_POINT ( 'NONE',  ( 54.51779242482700027, 32.54502000000000095, -30.64740209392260084 ) ) ;
#18627 = CARTESIAN_POINT ( 'NONE',  ( 5.776492041582129922, 11.58109048093756321, 0.6221623434578115175 ) ) ;
#18629 = ORIENTED_EDGE ( 'NONE', *, *, #13340, .F. ) ;
#18630 = CARTESIAN_POINT ( 'NONE',  ( 5.097018562294259425, 21.39650696725259849, 2.300254011810204613 ) ) ;
#18631 = DIRECTION ( 'NONE',  ( 0.08420877549337300871, 0.000000000000000000, 0.9964481331860212121 ) ) ;
#18632 = AXIS2_PLACEMENT_3D ( 'NONE', #14296, #10948, #17260 ) ;
#18633 = VERTEX_POINT ( 'NONE', #21027 ) ;
#18634 = CARTESIAN_POINT ( 'NONE',  ( 27.40895291499714403, -1.983739999999999837, -9.088367920799473865 ) ) ;
#18635 = ORIENTED_EDGE ( 'NONE', *, *, #12589, .F. ) ;
#18636 = DIRECTION ( 'NONE',  ( 0.000000000000000000, -1.000000000000000000, -0.000000000000000000 ) ) ;
#18637 = CARTESIAN_POINT ( 'NONE',  ( 30.97944403357121956, 34.52875999999999834, -8.103300075789407586 ) ) ;
#18638 = DIRECTION ( 'NONE',  ( 0.9237641507921645623, 0.000000000000000000, 0.3829618697876213673 ) ) ;
#18639 = CARTESIAN_POINT ( 'NONE',  ( 1.709033155221383993, 13.94841408984046005, -0.1006121354318848110 ) ) ;
#18640 = CARTESIAN_POINT ( 'NONE',  ( 1.954387715434429795, 8.736780638212259475, 10.71562499999999929 ) ) ;
#18641 = ORIENTED_EDGE ( 'NONE', *, *, #15466, .F. ) ;
#18642 = DIRECTION ( 'NONE',  ( 0.000000000000000000, 1.000000000000000000, -0.000000000000000000 ) ) ;
#18643 = CARTESIAN_POINT ( 'NONE',  ( 29.64606458365116737, 30.55334249999999940, -15.53894806404596096 ) ) ;
#18644 = CARTESIAN_POINT ( 'NONE',  ( 19.79515554403045741, 36.51313500000000545, -10.69562145279641996 ) ) ;
#18645 = CARTESIAN_POINT ( 'NONE',  ( 27.40895291499714403, 0.000000000000000000, -9.088367920799473865 ) ) ;
#18647 = CARTESIAN_POINT ( 'NONE',  ( 12.71652186471789037, -5.931147806008448597, -15.53286060487739029 ) ) ;
#18646 = DIRECTION ( 'NONE',  ( 0.000000000000000000, 1.000000000000000000, 0.000000000000000000 ) ) ;
#18648 = ORIENTED_EDGE ( 'NONE', *, *, #13057, .F. ) ;
#18649 = ORIENTED_EDGE ( 'NONE', *, *, #15336, .T. ) ;
#18650 = EDGE_CURVE ( 'NONE', #10775, #21819, #10643, .T. ) ;
#18651 = CARTESIAN_POINT ( 'NONE',  ( 13.22581436452122539, 21.49735766717988383, 2.368128691676176345 ) ) ;
#18652 = AXIS2_PLACEMENT_3D ( 'NONE', #12287, #5303, #1992 ) ;
#18654 = CARTESIAN_POINT ( 'NONE',  ( 9.907371917564091746, 34.52875999999999834, -13.23786778167655243 ) ) ;
#18653 = CARTESIAN_POINT ( 'NONE',  ( 4.693615291679356538, 20.53859366438406298, 6.837946208588576269 ) ) ;
#18655 = ORIENTED_EDGE ( 'NONE', *, *, #8520, .T. ) ;
#18656 = ORIENTED_EDGE ( 'NONE', *, *, #14919, .T. ) ;
#18657 = CARTESIAN_POINT ( 'NONE',  ( 29.76562500000000000, 0.000000000000000000, -4.317999999999999616 ) ) ;
#18658 = VERTEX_POINT ( 'NONE', #17396 ) ;
#18659 = CARTESIAN_POINT ( 'NONE',  ( 7.569648848239395100, 13.31117041489053499, -1.062061557284633473 ) ) ;
#18660 = VECTOR ( 'NONE', #20198, 1000.000000000000114 ) ;
#18661 = ADVANCED_FACE ( 'NONE', ( #12533 ), #800, .F. ) ;
#18662 = AXIS2_PLACEMENT_3D ( 'NONE', #694, #9421, #16194 ) ;
#18663 = FACE_OUTER_BOUND ( 'NONE', #17121, .T. ) ;
#18664 = CARTESIAN_POINT ( 'NONE',  ( -4.728951812473551897, 3.961447500000001565, -29.02782796843600011 ) ) ;
#18665 = CARTESIAN_POINT ( 'NONE',  ( 0.1350596924166655444, 12.33293199756963077, 2.070595033201866109 ) ) ;
#18666 = CARTESIAN_POINT ( 'NONE',  ( 30.24348838687780727, 32.54502000000000095, -20.27293523655082552 ) ) ;
#18667 = VERTEX_POINT ( 'NONE', #19257 ) ;
#18668 = CARTESIAN_POINT ( 'NONE',  ( 3.775593739218882749, 14.94275550331619229, 8.308998658764112477 ) ) ;
#18669 = CARTESIAN_POINT ( 'NONE',  ( 61.09555596642878328, 32.54502000000000095, -12.53419992421059348 ) ) ;
#18670 = CARTESIAN_POINT ( 'NONE',  ( 52.43275354619881057, -5.626267736715355738, -17.37840939435159981 ) ) ;
#18671 = ORIENTED_EDGE ( 'NONE', *, *, #149, .T. ) ;
#18672 = EDGE_CURVE ( 'NONE', #19005, #6777, #3, .T. ) ;
#18673 = CARTESIAN_POINT ( 'NONE',  ( 7.162339363255674662, 18.34001794662099982, -2.492660041346614896 ) ) ;
#18674 = AXIS2_PLACEMENT_3D ( 'NONE', #12563, #17635, #21157 ) ;
#18675 = EDGE_CURVE ( 'NONE', #6476, #12607, #3790, .T. ) ;
#18676 = ADVANCED_FACE ( 'NONE', ( #10526 ), #4013, .T. ) ;
#18677 = CARTESIAN_POINT ( 'NONE',  ( 13.38176279160079396, 15.86059960773468092, 7.158817725216849226 ) ) ;
#18678 = EDGE_LOOP ( 'NONE', ( #12002, #1973, #21539 ) ) ;
#18679 = PRODUCT_DEFINITION_SHAPE ( 'NONE', 'NONE',  #21889 ) ;
#18680 = ORIENTED_EDGE ( 'NONE', *, *, #20264, .F. ) ;
#18681 = CARTESIAN_POINT ( 'NONE',  ( -16.07247711516169275, -2.588178535606159958, -10.44681224123558039 ) ) ;
#18682 = CIRCLE ( 'NONE', #14836, 0.7950200000000003930 ) ;
#18683 = CARTESIAN_POINT ( 'NONE',  ( 9.381748681430247316, 13.20209339969382079, 7.058320365009602249 ) ) ;
#18684 = CARTESIAN_POINT ( 'NONE',  ( 5.070112026744222788, 20.64273285859446361, 2.209479276278648818 ) ) ;
#18685 = DIRECTION ( 'NONE',  ( -0.2490110332224849676, 0.000000000000000000, 0.9685006480810792739 ) ) ;
#18686 = VECTOR ( 'NONE', #6554, 1000.000000000000000 ) ;
#18687 = FACE_OUTER_BOUND ( 'NONE', #11166, .T. ) ;
#18688 = LINE ( 'NONE', #10, #11109 ) ;
#18689 = CARTESIAN_POINT ( 'NONE',  ( 9.699271717935820547, 13.10471967957858119, 6.517988425085752269 ) ) ;
#18690 = CARTESIAN_POINT ( 'NONE',  ( 5.375212648061713949, 14.86102846204294714, 7.798069169802851697 ) ) ;
#18691 = EDGE_CURVE ( 'NONE', #9393, #8373, #8128, .T. ) ;
#18692 = DIRECTION ( 'NONE',  ( 1.000000000000000000, 0.000000000000000000, 0.000000000000000000 ) ) ;
#18693 = CARTESIAN_POINT ( 'NONE',  ( 7.665089006313953846, 14.71660677864375799, 8.243516518557306938 ) ) ;
#18694 = CARTESIAN_POINT ( 'NONE',  ( 47.80475250345301674, -6.356984999999999886, -11.91473563638243327 ) ) ;
#18695 = PRODUCT_DEFINITION ( 'UNKNOWN', '', #8057, #7011 ) ;
#18696 = LINE ( 'NONE', #3565, #1842 ) ;
#18697 = VECTOR ( 'NONE', #16489, 1000.000000000000114 ) ;
#18698 = CARTESIAN_POINT ( 'NONE',  ( 2.063750000000000195, 30.56076406250000232, 10.71562496029980061 ) ) ;
#18699 = CARTESIAN_POINT ( 'NONE',  ( -2.234700160307072192, 3.961447500000001565, -24.80708529208898483 ) ) ;
#18700 = DIRECTION ( 'NONE',  ( -0.9964481331860212121, 0.000000000000000000, 0.08420877549337305035 ) ) ;
#18701 = CARTESIAN_POINT ( 'NONE',  ( 10.72385252731403860, -3.032576214141862625, -17.12574345756441119 ) ) ;
#18702 = VECTOR ( 'NONE', #213, 1000.000000000000114 ) ;
#18703 = DIRECTION ( 'NONE',  ( -0.000000000000000000, -1.000000000000000000, 0.000000000000000000 ) ) ;
#18704 = FACE_OUTER_BOUND ( 'NONE', #10506, .T. ) ;
#18705 = EDGE_CURVE ( 'NONE', #19184, #5628, #5433, .T. ) ;
#18706 = CARTESIAN_POINT ( 'NONE',  ( 11.35402150168352620, 17.07583819629140720, 7.537287116278762689 ) ) ;
#18707 = CARTESIAN_POINT ( 'NONE',  ( 14.25617145423489696, 36.51313500000000545, -15.80779474975094168 ) ) ;
#18708 = CARTESIAN_POINT ( 'NONE',  ( 12.67900527298905367, 11.74404568948788175, 3.672993509785967170 ) ) ;
#18709 = LINE ( 'NONE', #11980, #13745 ) ;
#18711 = DIRECTION ( 'NONE',  ( 0.000000000000000000, -1.000000000000000000, -0.000000000000000000 ) ) ;
#18710 = CARTESIAN_POINT ( 'NONE',  ( 2.545705333780837520, 11.94763405986570071, 5.186584416886813820 ) ) ;
#18712 = EDGE_LOOP ( 'NONE', ( #3039, #10933, #19316, #12011, #15175, #12488, #6671, #16610, #21523, #8137, #7460, #10375, #19879, #3012, #17283, #1962, #10875, #12699 ) ) ;
#18713 =( NAMED_UNIT ( * ) PLANE_ANGLE_UNIT ( ) SI_UNIT ( $, .RADIAN. ) );
#18714 = LINE ( 'NONE', #10208, #9562 ) ;
#18715 = DIRECTION ( 'NONE',  ( -0.2064631973582987667, 0.000000000000000000, 0.9784543669157944601 ) ) ;
#18716 = CARTESIAN_POINT ( 'NONE',  ( 6.239172611192463691, 10.95050572681988044, 2.838845822508675898 ) ) ;
#18717 = AXIS2_PLACEMENT_3D ( 'NONE', #11462, #4604, #14693 ) ;
#18718 = ORIENTED_EDGE ( 'NONE', *, *, #1907, .T. ) ;
#18719 = CARTESIAN_POINT ( 'NONE',  ( 7.404266004599425521, 14.64998413227717577, -1.914972092386549418 ) ) ;
#18720 = CARTESIAN_POINT ( 'NONE',  ( 3.982060119604976745, 20.45969085187979175, 4.972192302677306053 ) ) ;
#18721 = EDGE_CURVE ( 'NONE', #16113, #4424, #5658, .T. ) ;
#18722 = CARTESIAN_POINT ( 'NONE',  ( 7.439896507631877931, 14.64998413227717577, -1.925642189551348915 ) ) ;
#18723 = CARTESIAN_POINT ( 'NONE',  ( 3.865727471797527404, 21.04679274153226132, 3.426517514587319457 ) ) ;
#18724 = ADVANCED_FACE ( 'NONE', ( #18920 ), #2236, .F. ) ;
#18725 = EDGE_CURVE ( 'NONE', #4163, #14616, #16954, .T. ) ;
#18726 = AXIS2_PLACEMENT_3D ( 'NONE', #18851, #5470, #8458 ) ;
#18727 = CARTESIAN_POINT ( 'NONE',  ( 65.90927232300019512, 0.000000000000000000, -13.30734117861468135 ) ) ;
#18728 = CARTESIAN_POINT ( 'NONE',  ( 15.39982685781387239, -7.202102660715429039, -16.20421384448473745 ) ) ;
#18729 = UNCERTAINTY_MEASURE_WITH_UNIT (LENGTH_MEASURE( 1.000000000000000082E-05 ), #8229, 'distance_accuracy_value', 'NONE');
#18730 = LINE ( 'NONE', #12117, #12730 ) ;
#18731 = EDGE_LOOP ( 'NONE', ( #870, #17034, #18444, #714 ) ) ;
#18732 = CARTESIAN_POINT ( 'NONE',  ( 11.21471861299752248, 14.75766247937585618, 6.567071003333057710 ) ) ;
#18733 = CARTESIAN_POINT ( 'NONE',  ( 7.220654365899250138, 14.38088390058819144, -2.657754341408458565 ) ) ;
#18734 = VERTEX_POINT ( 'NONE', #7547 ) ;
#18735 = CARTESIAN_POINT ( 'NONE',  ( 66.03921914090641110, 32.54502000000000095, -11.33033647675950029 ) ) ;
#18736 = DIRECTION ( 'NONE',  ( 0.000000000000000000, -1.000000000000000000, 0.000000000000000000 ) ) ;
#18738 = CARTESIAN_POINT ( 'NONE',  ( 12.88040283537677588, 20.23395749999999893, -0.09070320285213756550 ) ) ;
#18737 = CARTESIAN_POINT ( 'NONE',  ( 5.301985385782669979, 15.65151869617330682, 8.867093223034917315 ) ) ;
#18739 = EDGE_LOOP ( 'NONE', ( #16196, #7382 ) ) ;
#18740 = CARTESIAN_POINT ( 'NONE',  ( 7.038019125744845006, 11.55073413761267176, 5.606060742231384175 ) ) ;
#18741 = CIRCLE ( 'NONE', #1082, 9.524999999999998579 ) ;
#18742 = AXIS2_PLACEMENT_3D ( 'NONE', #4608, #15020, #11350 ) ;
#18743 = VERTEX_POINT ( 'NONE', #2682 ) ;
#18744 = VECTOR ( 'NONE', #14886, 1000.000000000000114 ) ;
#18745 = CARTESIAN_POINT ( 'NONE',  ( 8.505511374756364873, 39.28205249999999893, -20.97439202360551747 ) ) ;
#18746 = VERTEX_POINT ( 'NONE', #13190 ) ;
#18747 =( GEOMETRIC_REPRESENTATION_CONTEXT ( 3 ) GLOBAL_UNCERTAINTY_ASSIGNED_CONTEXT ( ( #12326 ) ) GLOBAL_UNIT_ASSIGNED_CONTEXT ( ( #3461, #21806, #5215 ) ) REPRESENTATION_CONTEXT ( 'NONE', 'WORKASPACE' ) );
#18748 = EDGE_CURVE ( 'NONE', #1617, #4527, #16619, .T. ) ;
#18749 = CARTESIAN_POINT ( 'NONE',  ( 3.878057801843542762, 13.31387814151853100, 0.5091637933335767530 ) ) ;
#18750 = PLANE ( 'NONE',  #11750 ) ;
#18751 = DIRECTION ( 'NONE',  ( 0.000000000000000000, 1.000000000000000000, 0.000000000000000000 ) ) ;
#18752 = LINE ( 'NONE', #15248, #8658 ) ;
#18753 = CARTESIAN_POINT ( 'NONE',  ( 38.82016491058538321, -9.531985000000000596, -14.75770094105646812 ) ) ;
#18754 = AXIS2_PLACEMENT_3D ( 'NONE', #17936, #8296, #13301 ) ;
#18755 = AXIS2_PLACEMENT_3D ( 'NONE', #1879, #8626, #15403 ) ;
#18756 = EDGE_LOOP ( 'NONE', ( #3292, #16220, #20495, #8910 ) ) ;
#18757 = LINE ( 'NONE', #11703, #21639 ) ;
#18758 = DIRECTION ( 'NONE',  ( 0.000000000000000000, 1.000000000000000000, 0.000000000000000000 ) ) ;
#18759 = FACE_OUTER_BOUND ( 'NONE', #13733, .T. ) ;
#18761 = CARTESIAN_POINT ( 'NONE',  ( 12.23724559180106297, -5.318041355315282992, -15.61933097726557662 ) ) ;
#18760 = LINE ( 'NONE', #5385, #9502 ) ;
#18762 = ORIENTED_EDGE ( 'NONE', *, *, #9120, .T. ) ;
#18763 = ORIENTED_EDGE ( 'NONE', *, *, #3508, .T. ) ;
#18764 = AXIS2_PLACEMENT_3D ( 'NONE', #13507, #8188, #18351 ) ;
#18765 = CARTESIAN_POINT ( 'NONE',  ( 11.11804983913708789, 14.04693538215814108, 6.410641060063417385 ) ) ;
#18766 = CARTESIAN_POINT ( 'NONE',  ( 4.613777796174654888, 10.97171856713620031, 3.809597102348731834 ) ) ;
#18767 = ORIENTED_EDGE ( 'NONE', *, *, #4298, .T. ) ;
#18768 = VERTEX_POINT ( 'NONE', #11288 ) ;
#18769 = CARTESIAN_POINT ( 'NONE',  ( -17.46249999999999858, 0.000000000000000000, 0.000000000000000000 ) ) ;
#18770 = EDGE_LOOP ( 'NONE', ( #1620, #18228, #11137, #10023 ) ) ;
#18771 = CARTESIAN_POINT ( 'NONE',  ( 7.622376558701811966, 12.99890566801571801, -0.7894648885981262465 ) ) ;
#18772 = VECTOR ( 'NONE', #10830, 1000.000000000000000 ) ;
#18773 = AXIS2_PLACEMENT_3D ( 'NONE', #13940, #10258, #2067 ) ;
#18774 = ORIENTED_EDGE ( 'NONE', *, *, #20331, .T. ) ;
#18775 = EDGE_CURVE ( 'NONE', #1384, #12537, #1006, .T. ) ;
#18776 = AXIS2_PLACEMENT_3D ( 'NONE', #8591, #16997, #21651 ) ;
#18777 = CIRCLE ( 'NONE', #2186, 1.587500000000001688 ) ;
#18778 = DIRECTION ( 'NONE',  ( 0.000000000000000000, -1.000000000000000000, 0.000000000000000000 ) ) ;
#18779 = CYLINDRICAL_SURFACE ( 'NONE', #2287, 1.191259999999998209 ) ;
#18780 = CARTESIAN_POINT ( 'NONE',  ( 0.7990183446076977170, 20.43784215561237616, 2.136429022385333720 ) ) ;
#18781 = EDGE_LOOP ( 'NONE', ( #15689, #2962, #9083, #15151 ) ) ;
#18782 = CARTESIAN_POINT ( 'NONE',  ( 0.5202139640632184037, 20.26160593876955929, 6.118137731981865279 ) ) ;
#18783 = CARTESIAN_POINT ( 'NONE',  ( -51.02421882195815783, 38.25938500000000175, -23.02637480153789795 ) ) ;
#18784 = DIRECTION ( 'NONE',  ( 0.000000000000000000, -1.000000000000000000, -0.000000000000000000 ) ) ;
#18785 = DIRECTION ( 'NONE',  ( 0.9579671649362032637, 0.000000000000000000, -0.2868778675745010664 ) ) ;
#18786 = VECTOR ( 'NONE', #10036, 1000.000000000000000 ) ;
#18787 = ORIENTED_EDGE ( 'NONE', *, *, #4494, .F. ) ;
#18788 = CARTESIAN_POINT ( 'NONE',  ( 6.472117061228174428, 11.13551934581288094, 4.539831998221737663 ) ) ;
#18789 = CARTESIAN_POINT ( 'NONE',  ( 50.62387473582167274, 32.54502000000000095, -28.41576006634952734 ) ) ;
#18790 = CARTESIAN_POINT ( 'NONE',  ( 10.98481630133226972, 22.00956135593990126, 1.091099386501859891 ) ) ;
#18791 = ORIENTED_EDGE ( 'NONE', *, *, #12901, .T. ) ;
#18792 = DIRECTION ( 'NONE',  ( -0.9685006480810794960, 0.000000000000000000, -0.2490110332224836354 ) ) ;
#18793 = ORIENTED_EDGE ( 'NONE', *, *, #3188, .F. ) ;
#18794 = DIRECTION ( 'NONE',  ( 0.000000000000000000, 1.000000000000000000, 0.000000000000000000 ) ) ;
#18795 = CARTESIAN_POINT ( 'NONE',  ( 9.257010659763754035, 12.43204336432666679, 6.443182332374063570 ) ) ;
#18796 = CIRCLE ( 'NONE', #19152, 1.984374999999998890 ) ;
#18797 = CARTESIAN_POINT ( 'NONE',  ( 4.600923355963855599, 11.78113229454884170, 3.799008705536232711 ) ) ;
#18798 = CARTESIAN_POINT ( 'NONE',  ( 42.79471501377724252, 0.000000000000000000, 5.049205022181460834 ) ) ;
#18799 = EDGE_CURVE ( 'NONE', #1021, #7386, #12972, .T. ) ;
#18800 = CARTESIAN_POINT ( 'NONE',  ( 5.758048114252814820, 17.57362948320378493, -1.250247827883776974 ) ) ;
#18801 = CARTESIAN_POINT ( 'NONE',  ( 67.40134256979101224, 1.984375000000000000, -13.70358117861468017 ) ) ;
#18802 = VECTOR ( 'NONE', #5262, 1000.000000000000000 ) ;
#18803 = ADVANCED_FACE ( 'NONE', ( #8074 ), #14163, .T. ) ;
#18804 = CARTESIAN_POINT ( 'NONE',  ( 14.59117433460712476, 20.92287966070258065, 3.915742219214028541 ) ) ;
#18805 = EDGE_CURVE ( 'NONE', #3173, #13394, #7078, .T. ) ;
#18806 = CARTESIAN_POINT ( 'NONE',  ( 5.189412234176333349, 13.04569946892264198, 6.627088851125058966 ) ) ;
#18807 = CARTESIAN_POINT ( 'NONE',  ( -0.3434148217290114435, 21.11429744052310298, 4.777665891053347380 ) ) ;
#18808 = CARTESIAN_POINT ( 'NONE',  ( -22.90765545213488963, -6.903720000000000745, -9.869178565316103047 ) ) ;
#18809 = VECTOR ( 'NONE', #16420, 1000.000000000000000 ) ;
#18810 = CYLINDRICAL_SURFACE ( 'NONE', #6800, 0.7950199999999993938 ) ;
#18811 = CARTESIAN_POINT ( 'NONE',  ( 6.380166963026771221, 10.92343582149830183, 2.794643371853744007 ) ) ;
#18812 = FACE_OUTER_BOUND ( 'NONE', #1164, .T. ) ;
#18813 = DIRECTION ( 'NONE',  ( 0.000000000000000000, 1.000000000000000000, 0.000000000000000000 ) ) ;
#18814 = CARTESIAN_POINT ( 'NONE',  ( 18.88804190845695530, -7.531632358019679785, -15.45048948743678352 ) ) ;
#18815 = DIRECTION ( 'NONE',  ( 0.000000000000000000, 1.000000000000000000, 0.000000000000000000 ) ) ;
#18816 = CARTESIAN_POINT ( 'NONE',  ( 38.60701496492545459, 34.52875999999999834, -26.94161103631838472 ) ) ;
#18817 = CARTESIAN_POINT ( 'NONE',  ( 11.19012038083658567, 18.30292129351066777, 7.238227121531449981 ) ) ;
#18818 = LINE ( 'NONE', #3686, #15083 ) ;
#18819 = CIRCLE ( 'NONE', #4020, 0.3962399999999999811 ) ;
#18820 = CARTESIAN_POINT ( 'NONE',  ( 42.66304184606194383, -1.983739999999999837, -19.22597499813143784 ) ) ;
#18821 = CARTESIAN_POINT ( 'NONE',  ( 11.16285581286486916, 14.48099254937300095, -3.237536915232507528 ) ) ;
#18822 = CARTESIAN_POINT ( 'NONE',  ( 22.02657784715807665, 34.52875999999999834, -12.98906981665815330 ) ) ;
#18824 = CARTESIAN_POINT ( 'NONE',  ( 1.173720826352361080, -1.594802499999999013, -20.82884779549221577 ) ) ;
#18823 = CARTESIAN_POINT ( 'NONE',  ( 2.203866969713045076, 11.92572550326888070, 3.650552894295490347 ) ) ;
#18825 = ORIENTED_EDGE ( 'NONE', *, *, #1948, .F. ) ;
#18826 = APPLICATION_PROTOCOL_DEFINITION ( 'draft international standard', 'automotive_design', 1998, #4393 ) ;
#18827 = EDGE_CURVE ( 'NONE', #2587, #10772, #19410, .T. ) ;
#18828 = CARTESIAN_POINT ( 'NONE',  ( -24.20935654380574320, -6.905625000000000568, -25.29247038871795894 ) ) ;
#18829 = AXIS2_PLACEMENT_3D ( 'NONE', #8405, #15412, #10183 ) ;
#18830 = CARTESIAN_POINT ( 'NONE',  ( 6.189386483567429487, 11.65214456485618300, 2.904983884989000398 ) ) ;
#18831 = EDGE_LOOP ( 'NONE', ( #15926, #14368, #8049, #2489 ) ) ;
#18832 = CARTESIAN_POINT ( 'NONE',  ( 11.07392898271076120, 17.51362067755397334, 6.788261054904052294 ) ) ;
#18833 = EDGE_CURVE ( 'NONE', #7807, #10315, #4549, .T. ) ;
#18834 = AXIS2_PLACEMENT_3D ( 'NONE', #18343, #3209, #10271 ) ;
#18835 = CARTESIAN_POINT ( 'NONE',  ( 11.62621442616514678, 11.69902548067542192, -0.9660039452025425133 ) ) ;
#18836 = CARTESIAN_POINT ( 'NONE',  ( 0.6791493861838465707, 11.70670645901422091, 3.098048504804435055 ) ) ;
#18837 = CARTESIAN_POINT ( 'NONE',  ( 13.39304148437000386, 14.65557762784733598, 7.068600972872675747 ) ) ;
#18838 = DIRECTION ( 'NONE',  ( 0.000000000000000000, 1.000000000000000000, 0.000000000000000000 ) ) ;
#18839 = ADVANCED_FACE ( 'NONE', ( #21564 ), #21449, .T. ) ;
#18840 = CARTESIAN_POINT ( 'NONE',  ( 15.27944507982620692, 1.059665764626953388, -15.67595978355573116 ) ) ;
#18841 = LINE ( 'NONE', #10450, #17662 ) ;
#18842 = EDGE_LOOP ( 'NONE', ( #10201, #6106, #14456, #6599, #1157, #1317, #4772, #1504, #4753, #11010, #3656, #10808, #3511, #3618, #7262, #15682, #9013, #7738 ) ) ;
#18843 = CARTESIAN_POINT ( 'NONE',  ( 11.19568187662517467, 16.10043549507820870, 6.812789942806879218 ) ) ;
#18844 = CARTESIAN_POINT ( 'NONE',  ( 11.99126722525327082, 10.32956393789710070, 0.6475472086173773567 ) ) ;
#18845 = AXIS2_PLACEMENT_3D ( 'NONE', #10751, #1000, #19893 ) ;
#18846 = EDGE_LOOP ( 'NONE', ( #14334, #19991, #10624, #2281 ) ) ;
#18847 = CARTESIAN_POINT ( 'NONE',  ( 9.313964464681076194, 14.38829612573348093, -2.460586518476112872 ) ) ;
#18848 = CARTESIAN_POINT ( 'NONE',  ( 8.505511374756364873, 6.343967500000000648, -20.97439202360551747 ) ) ;
#18849 = CARTESIAN_POINT ( 'NONE',  ( -22.70813868260604096, -0.3962399999999990929, 1.090609736204201763 ) ) ;
#18851 = CARTESIAN_POINT ( 'NONE',  ( 26.59920545652001067, 26.98019749999999917, -43.69048495915765074 ) ) ;
#18850 = CARTESIAN_POINT ( 'NONE',  ( 5.976523806576305553, 21.10281604008488188, 5.596071939254449568 ) ) ;
#18852 = ORIENTED_EDGE ( 'NONE', *, *, #21666, .T. ) ;
#18853 = CARTESIAN_POINT ( 'NONE',  ( 6.380166963026771221, 10.92343582149830183, 2.794643371853744007 ) ) ;
#18854 = EDGE_CURVE ( 'NONE', #13538, #3590, #5998, .T. ) ;
#18855 = AXIS2_PLACEMENT_3D ( 'NONE', #4847, #4743, #7250 ) ;
#18856 = ADVANCED_FACE ( 'NONE', ( #2894 ), #2780, .F. ) ;
#18857 = DIRECTION ( 'NONE',  ( 0.000000000000000000, -1.000000000000000000, 0.000000000000000000 ) ) ;
#18858 = EDGE_CURVE ( 'NONE', #4163, #15435, #17307, .T. ) ;
#18859 = VERTEX_POINT ( 'NONE', #4661 ) ;
#18860 = CARTESIAN_POINT ( 'NONE',  ( 0.4780069470470488802, 12.44023573197847199, 3.531212066111156123 ) ) ;
#18861 = VERTEX_POINT ( 'NONE', #19900 ) ;
#18862 = AXIS2_PLACEMENT_3D ( 'NONE', #1668, #11959, #11856 ) ;
#18863 = DIRECTION ( 'NONE',  ( 0.000000000000000000, 1.000000000000000000, 0.000000000000000000 ) ) ;
#18864 = CARTESIAN_POINT ( 'NONE',  ( -13.87568970999206108, -1.983739999999999393, -9.457638332870221376 ) ) ;
#18865 = VECTOR ( 'NONE', #14057, 1000.000000000000114 ) ;
#18866 = CARTESIAN_POINT ( 'NONE',  ( 12.25799425556778388, 36.51313500000000545, 0.2069032437451798767 ) ) ;
#18867 = CARTESIAN_POINT ( 'NONE',  ( 5.434136948886521878, 17.60830669131005877, 8.646509754689903460 ) ) ;
#18868 = CARTESIAN_POINT ( 'NONE',  ( 55.14150854986954897, 38.88803500000000213, -23.45621182681304617 ) ) ;
#18869 = ORIENTED_EDGE ( 'NONE', *, *, #9116, .T. ) ;
#18870 = LINE ( 'NONE', #7274, #13920 ) ;
#18871 = DIRECTION ( 'NONE',  ( 0.000000000000000000, -1.000000000000000000, 0.000000000000000000 ) ) ;
#18872 = FILL_AREA_STYLE ('',( #8592 ) ) ;
#18874 = CARTESIAN_POINT ( 'NONE',  ( 14.48894653437083058, -7.059436537805347633, -15.17821728035911910 ) ) ;
#18873 = CARTESIAN_POINT ( 'NONE',  ( -20.63749999999999929, 16.27314499999999953, 8.731249999999999289 ) ) ;
#18875 = ORIENTED_EDGE ( 'NONE', *, *, #16116, .T. ) ;
#18876 = ORIENTED_EDGE ( 'NONE', *, *, #13563, .T. ) ;
#18877 = CARTESIAN_POINT ( 'NONE',  ( 5.700318986066064575, 17.24315932450417321, -1.422019646414491856 ) ) ;
#18879 = PLANE ( 'NONE',  #3604 ) ;
#18878 = CARTESIAN_POINT ( 'NONE',  ( 4.099623927830029047, 21.31561936814513913, 5.248974889739956851 ) ) ;
#18880 = ORIENTED_EDGE ( 'NONE', *, *, #19135, .T. ) ;
#18881 = CARTESIAN_POINT ( 'NONE',  ( 4.703503668085327050, 11.11441527681874142, 4.315609331493701184 ) ) ;
#18882 = ORIENTED_EDGE ( 'NONE', *, *, #21103, .F. ) ;
#18883 = EDGE_CURVE ( 'NONE', #18557, #18658, #3900, .T. ) ;
#18884 = ORIENTED_EDGE ( 'NONE', *, *, #6544, .T. ) ;
#18885 = CARTESIAN_POINT ( 'NONE',  ( 7.888376708752765865, 12.04261116452797609, 0.4714777786467096998 ) ) ;
#18886 = AXIS2_PLACEMENT_3D ( 'NONE', #16206, #2702, #15573 ) ;
#18887 = ORIENTED_EDGE ( 'NONE', *, *, #6650, .T. ) ;
#18888 = DIRECTION ( 'NONE',  ( 0.000000000000000000, 1.000000000000000000, 0.000000000000000000 ) ) ;
#18889 = CARTESIAN_POINT ( 'NONE',  ( 67.40134256979101224, 74.97070807199999365, -13.70358117861468017 ) ) ;
#18890 = CARTESIAN_POINT ( 'NONE',  ( 41.45112526417833010, 34.52875999999999834, 7.778260066349530710 ) ) ;
#18891 = CARTESIAN_POINT ( 'NONE',  ( 2.888697626805730945, 19.94910490213707277, 7.692677454159938755 ) ) ;
#18892 = CARTESIAN_POINT ( 'NONE',  ( 8.011380105705496746, 24.59767750000000319, -19.05252355006962617 ) ) ;
#18893 = EDGE_LOOP ( 'NONE', ( #19084, #16601, #11937, #8809 ) ) ;
#18894 = CARTESIAN_POINT ( 'NONE',  ( 5.517512485557888091, 12.88680353640996223, 6.629587463472963904 ) ) ;
#18895 = DIRECTION ( 'NONE',  ( -0.7421532822901579785, 0.000000000000000000, 0.6702301885068630005 ) ) ;
#18896 = DIRECTION ( 'NONE',  ( -0.9964481331860213231, 0.000000000000000000, 0.08420877549337293932 ) ) ;
#18897 = DIRECTION ( 'NONE',  ( 0.8609107660235850723, 0.000000000000000000, -0.5087559856598092844 ) ) ;
#18898 = VECTOR ( 'NONE', #4801, 1000.000000000000114 ) ;
#18899 = ORIENTED_EDGE ( 'NONE', *, *, #7242, .T. ) ;
#18900 = CARTESIAN_POINT ( 'NONE',  ( 6.943297528318779221, 16.37851731477712391, -2.829567754717221106 ) ) ;
#18901 = DIRECTION ( 'NONE',  ( 0.05085730733808393328, 0.000000000000000000, -0.9987059298363656357 ) ) ;
#18902 = CARTESIAN_POINT ( 'NONE',  ( 11.23807322027795941, 22.05295773698684059, 1.794423719884019608 ) ) ;
#18903 = ORIENTED_EDGE ( 'NONE', *, *, #18561, .T. ) ;
#18904 = VERTEX_POINT ( 'NONE', #11505 ) ;
#18905 = EDGE_CURVE ( 'NONE', #17225, #10798, #15253, .T. ) ;
#18906 = DIRECTION ( 'NONE',  ( 0.000000000000000000, 1.000000000000000000, 0.000000000000000000 ) ) ;
#18907 = CARTESIAN_POINT ( 'NONE',  ( 9.444405600912201493, 16.57974156473798644, 7.980283251028787106 ) ) ;
#18908 = CARTESIAN_POINT ( 'NONE',  ( 4.978313727356318275, 18.75934072859504198, 7.426436322610240559 ) ) ;
#18909 = DIRECTION ( 'NONE',  ( -0.4987171968201928873, 0.000000000000000000, 0.8667647648559606566 ) ) ;
#18910 = CARTESIAN_POINT ( 'NONE',  ( 5.595240304620284100, 15.74558502937677851, -1.353109612183827304 ) ) ;
#18911 = CARTESIAN_POINT ( 'NONE',  ( 0.8982290014495240005, 19.73309768672615405, 2.485244984172155114 ) ) ;
#18912 = CARTESIAN_POINT ( 'NONE',  ( 38.96848998618624904, 40.07865999999999929, -3.934807454472129429 ) ) ;
#18913 = EDGE_CURVE ( 'NONE', #13013, #3881, #15262, .T. ) ;
#18914 = CARTESIAN_POINT ( 'NONE',  ( 10.71299524138181347, 20.94030016091612367, 5.223175413353787988 ) ) ;
#18915 = DIRECTION ( 'NONE',  ( 0.2868778675745011220, 0.000000000000000000, 0.9579671649362034858 ) ) ;
#18916 = CARTESIAN_POINT ( 'NONE',  ( -0.1852845025067436646, 13.90840449083211183, 0.5712815246737864561 ) ) ;
#18917 = CARTESIAN_POINT ( 'NONE',  ( 37.07154142533928365, -6.356984999999999886, -2.340318470350700508 ) ) ;
#18918 = CARTESIAN_POINT ( 'NONE',  ( 20.20352062662200154, -1.069946468824292563, -14.76680097212925347 ) ) ;
#18919 = DIRECTION ( 'NONE',  ( 0.2868778675745011220, 0.000000000000000000, 0.9579671649362034858 ) ) ;
#18920 = FACE_OUTER_BOUND ( 'NONE', #15457, .T. ) ;
#18921 = CYLINDRICAL_SURFACE ( 'NONE', #12933, 20.83593749999999289 ) ;
#18922 = CARTESIAN_POINT ( 'NONE',  ( 16.64770984238460372, 2.218310395241972266, -15.26570684048795457 ) ) ;
#18923 = FACE_OUTER_BOUND ( 'NONE', #18202, .T. ) ;
#18924 = CYLINDRICAL_SURFACE ( 'NONE', #20857, 30.16249999999999432 ) ;
#18925 = CARTESIAN_POINT ( 'NONE',  ( 10.28455556095842205, 21.13454001091563228, 4.959045466106354993 ) ) ;
#18926 = CARTESIAN_POINT ( 'NONE',  ( 30.41963056417667488, 34.52875999999999834, -8.653862521447852174 ) ) ;
#18927 = EDGE_CURVE ( 'NONE', #19208, #6484, #13145, .T. ) ;
#18928 = CARTESIAN_POINT ( 'NONE',  ( 11.22362340204833409, 13.65647046284849253, -2.836478600376960202 ) ) ;
#18929 = EDGE_CURVE ( 'NONE', #3364, #9466, #16912, .T. ) ;
#18930 = CARTESIAN_POINT ( 'NONE',  ( 53.46798503507454825, -1.983739999999999837, 6.304111036318381878 ) ) ;
#18931 = CARTESIAN_POINT ( 'NONE',  ( 7.076841547715329028, 14.92411314052326965, 7.692205025965034082 ) ) ;
#18932 = ORIENTED_EDGE ( 'NONE', *, *, #6354, .T. ) ;
#18933 = APPLICATION_PROTOCOL_DEFINITION ( 'draft international standard', 'automotive_design', 1998, #19766 ) ;
#18934 = DIRECTION ( 'NONE',  ( 0.9685006480810793850, 0.000000000000000000, 0.2490110332224846623 ) ) ;
#18935 = PLANE ( 'NONE',  #4757 ) ;
#18936 = ORIENTED_EDGE ( 'NONE', *, *, #4097, .T. ) ;
#18937 = CARTESIAN_POINT ( 'NONE',  ( 8.673696226316383928, 11.54146397052094208, 3.508390839460689303 ) ) ;
#18938 = CARTESIAN_POINT ( 'NONE',  ( 9.352043289815954452, 13.73224064219962592, -2.247542222848531779 ) ) ;
#18939 = CARTESIAN_POINT ( 'NONE',  ( 2.415895693004135314, 18.09708922108623241, -0.2312783618673834030 ) ) ;
#18940 = LINE ( 'NONE', #14224, #436 ) ;
#18941 = CARTESIAN_POINT ( 'NONE',  ( 39.62791084302666178, 0.000000000000000000, -24.65774797299118859 ) ) ;
#18942 = EDGE_CURVE ( 'NONE', #11378, #17699, #12780, .T. ) ;
#18943 = CARTESIAN_POINT ( 'NONE',  ( 18.85280999513622646, -0.3457920826010936199, -14.56172347197127692 ) ) ;
#18944 = UNCERTAINTY_MEASURE_WITH_UNIT (LENGTH_MEASURE( 1.000000000000000082E-05 ), #20231, 'distance_accuracy_value', 'NONE');
#18945 = LINE ( 'NONE', #10340, #1065 ) ;
#18946 = ORIENTED_EDGE ( 'NONE', *, *, #2345, .T. ) ;
#18947 = CARTESIAN_POINT ( 'NONE',  ( 11.20183242851396166, 15.98666862805646005, 6.807554364040996120 ) ) ;
#18948 = CARTESIAN_POINT ( 'NONE',  ( 10.93328336395047451, 14.15736234249478720, -4.068969855961862336 ) ) ;
#18949 = ORIENTED_EDGE ( 'NONE', *, *, #15365, .F. ) ;
#18950 = EDGE_CURVE ( 'NONE', #8103, #21087, #9832, .T. ) ;
#18951 = CARTESIAN_POINT ( 'NONE',  ( 9.574157909608086214, 12.48569481993280839, -1.056400077264328052 ) ) ;
#18952 = LINE ( 'NONE', #9552, #2853 ) ;
#18953 = DIRECTION ( 'NONE',  ( 0.000000000000000000, 1.000000000000000000, 0.000000000000000000 ) ) ;
#18954 = ADVANCED_FACE ( 'NONE', ( #20319 ), #1553, .T. ) ;
#18956 = DIRECTION ( 'NONE',  ( 0.000000000000000000, 1.000000000000000000, 0.000000000000000000 ) ) ;
#18955 = CARTESIAN_POINT ( 'NONE',  ( 4.694926625316558244, 21.33523753305656001, 2.105523894130039597 ) ) ;
#18957 = EDGE_LOOP ( 'NONE', ( #21562, #1179, #8675, #4233 ) ) ;
#18958 = CARTESIAN_POINT ( 'NONE',  ( 6.719255672218935160, 11.03203715683660135, 4.231726879825330911 ) ) ;
#18959 = CYLINDRICAL_SURFACE ( 'NONE', #7707, 0.7950200000000005041 ) ;
#18960 = VERTEX_POINT ( 'NONE', #5189 ) ;
#18961 = PLANE ( 'NONE',  #2973 ) ;
#18962 = AXIS2_PLACEMENT_3D ( 'NONE', #11824, #13061, #3198 ) ;
#18963 = CARTESIAN_POINT ( 'NONE',  ( 39.11079947626275555, 32.54502000000000095, -27.65534212225540500 ) ) ;
#18964 = ORIENTED_EDGE ( 'NONE', *, *, #19283, .T. ) ;
#18965 = CARTESIAN_POINT ( 'NONE',  ( 3.360635606688116894, 36.51313500000000545, -20.45316710734507026 ) ) ;
#18966 = FACE_OUTER_BOUND ( 'NONE', #2602, .T. ) ;
#18967 = CARTESIAN_POINT ( 'NONE',  ( -15.39353573898878658, -2.254660308866960339, -10.30107656633069979 ) ) ;
#18968 = EDGE_CURVE ( 'NONE', #8481, #3974, #20422, .T. ) ;
#18969 = CARTESIAN_POINT ( 'NONE',  ( 19.88300675555340291, -1.573955445284405785, -15.61985652438219496 ) ) ;
#18970 = CARTESIAN_POINT ( 'NONE',  ( 49.41195815393805901, 42.06303499999999929, -1.411525001868561224 ) ) ;
#18971 = PRODUCT_RELATED_PRODUCT_CATEGORY ( 'part', '', ( #17286 ) ) ;
#18972 = VERTEX_POINT ( 'NONE', #9953 ) ;
#18973 = CARTESIAN_POINT ( 'NONE',  ( 38.78586790977451670, 38.88803500000000213, -5.374168024304903035 ) ) ;
#18974 = CARTESIAN_POINT ( 'NONE',  ( 30.97944403357121956, 34.52875999999999834, -8.103300075789407586 ) ) ;
#18976 = CARTESIAN_POINT ( 'NONE',  ( 14.25617145423489696, 34.52875999999999834, -15.80779474975094168 ) ) ;
#18975 = DIRECTION ( 'NONE',  ( 1.000000000000000000, 0.000000000000000000, 0.000000000000000000 ) ) ;
#18977 = VERTEX_POINT ( 'NONE', #11938 ) ;
#18978 = ORIENTED_EDGE ( 'NONE', *, *, #19775, .T. ) ;
#18979 = CARTESIAN_POINT ( 'NONE',  ( 13.10461138620464361, 14.87610706663263826, 6.337233188073541967 ) ) ;
#18980 = AXIS2_PLACEMENT_3D ( 'NONE', #325, #15281, #18566 ) ;
#18982 = CYLINDRICAL_SURFACE ( 'NONE', #4670, 3.970019999999997662 ) ;
#18981 = CARTESIAN_POINT ( 'NONE',  ( 5.385071355335792731, 12.35064203674882144, 7.174237779700658457 ) ) ;
#18983 = ORIENTED_EDGE ( 'NONE', *, *, #19891, .T. ) ;
#18985 = CARTESIAN_POINT ( 'NONE',  ( 21.54912629262006973, -3.402682142040095670, -14.80437132354864715 ) ) ;
#18984 = CARTESIAN_POINT ( 'NONE',  ( 5.076974952998434709, 11.60801150508606128, 5.931021133774994958 ) ) ;
#18986 = ORIENTED_EDGE ( 'NONE', *, *, #21577, .F. ) ;
#18987 = ORIENTED_EDGE ( 'NONE', *, *, #7734, .T. ) ;
#18988 = CARTESIAN_POINT ( 'NONE',  ( 7.887801445722042004, 18.97569031398505146, -1.398027553882073004 ) ) ;
#18989 = CARTESIAN_POINT ( 'NONE',  ( 1.473177303762296608, 14.65264615020049099, 8.504923832329929212 ) ) ;
#18990 = VERTEX_POINT ( 'NONE', #15166 ) ;
#18991 = AXIS2_PLACEMENT_3D ( 'NONE', #17313, #283, #2040 ) ;
#18992 = CARTESIAN_POINT ( 'NONE',  ( 13.01576158600160049, 0.2519556637135220156, 9.701108553893439179 ) ) ;
#18993 = EDGE_CURVE ( 'NONE', #20988, #4180, #20156, .T. ) ;
#18994 = CARTESIAN_POINT ( 'NONE',  ( 38.55086098473930889, -7.409553547294740028, -4.428244049269694393 ) ) ;
#18995 = CARTESIAN_POINT ( 'NONE',  ( 49.81956284419040060, 1.984375000000000000, 11.98436472153758103 ) ) ;
#18996 = CARTESIAN_POINT ( 'NONE',  ( 1.401597142160411202, 21.11691655071049922, 3.736020553106880193 ) ) ;
#18997 = EDGE_CURVE ( 'NONE', #2302, #8192, #3947, .T. ) ;
#18998 = CARTESIAN_POINT ( 'NONE',  ( 0.000000000000000000, 32.54502000000000095, 0.000000000000000000 ) ) ;
#18999 = ORIENTED_EDGE ( 'NONE', *, *, #16908, .T. ) ;
#19000 = CARTESIAN_POINT ( 'NONE',  ( 4.384837209473736230, 18.74075759514924400, -0.3090233597782079400 ) ) ;
#19001 = LINE ( 'NONE', #12391, #13485 ) ;
#19002 = DIRECTION ( 'NONE',  ( 0.2490110332224850509, 0.000000000000000000, -0.9685006480810792739 ) ) ;
#19003 = CARTESIAN_POINT ( 'NONE',  ( 11.82678039945931481, -1.983739999999999393, -12.74436900065013667 ) ) ;
#19004 = ORIENTED_EDGE ( 'NONE', *, *, #2770, .F. ) ;
#19005 = VERTEX_POINT ( 'NONE', #15284 ) ;
#19006 = CARTESIAN_POINT ( 'NONE',  ( 5.147480976434583688, 17.32712159277285124, -1.670171097842100050 ) ) ;
#19007 = CARTESIAN_POINT ( 'NONE',  ( 39.07078961959606289, 34.52875999999999834, -27.14892015257980162 ) ) ;
#19008 = CARTESIAN_POINT ( 'NONE',  ( 12.47629024345491899, 10.55913518404749141, 2.732682640108681227 ) ) ;
#19009 = ORIENTED_EDGE ( 'NONE', *, *, #17087, .F. ) ;
#19010 = ORIENTED_EDGE ( 'NONE', *, *, #18177, .F. ) ;
#19011 = DIRECTION ( 'NONE',  ( -0.2868778675745011220, 0.000000000000000000, -0.9579671649362034858 ) ) ;
#19012 = AXIS2_PLACEMENT_3D ( 'NONE', #1233, #18572, #21452 ) ;
#19013 = CARTESIAN_POINT ( 'NONE',  ( 8.622933100223315606, 10.85996554133373060, 3.667822295698338397 ) ) ;
#19014 = CARTESIAN_POINT ( 'NONE',  ( 0.1620597292614394114, 17.19705222221691088, 0.7801052633530786151 ) ) ;
#19015 = CARTESIAN_POINT ( 'NONE',  ( 61.09555596642878328, 0.000000000000000000, -12.53419992421059348 ) ) ;
#19016 = CARTESIAN_POINT ( 'NONE',  ( 5.881467817102347340, 12.57312689154560736, 0.5107683554711034413 ) ) ;
#19017 = DIRECTION ( 'NONE',  ( 0.000000000000000000, 0.000000000000000000, 1.000000000000000000 ) ) ;
#19018 = CARTESIAN_POINT ( 'NONE',  ( -23.36909032872569014, 26.98019749999999917, -10.47372115209112842 ) ) ;
#19019 = CARTESIAN_POINT ( 'NONE',  ( 9.390327731862623040, 21.87018156742340125, 1.595481807788067030 ) ) ;
#19020 = DIRECTION ( 'NONE',  ( 0.000000000000000000, -1.000000000000000000, -0.000000000000000000 ) ) ;
#19021 = CARTESIAN_POINT ( 'NONE',  ( 44.27024749654656688, -5.166360000000000063, -8.722764363618033201 ) ) ;
#19022 = CARTESIAN_POINT ( 'NONE',  ( 0.2519962783006516327, 20.95646860120554322, 6.403714366392914137 ) ) ;
#19023 = DIRECTION ( 'NONE',  ( -0.9987059298363656357, 0.000000000000000000, -0.05085730733808393328 ) ) ;
#19024 = EDGE_CURVE ( 'NONE', #18977, #3969, #8179, .T. ) ;
#19025 = AXIS2_PLACEMENT_3D ( 'NONE', #21867, #6282, #4525 ) ;
#19026 = CARTESIAN_POINT ( 'NONE',  ( 20.23139908883704763, -1.200391101382722203, -14.75749743533480007 ) ) ;
#19027 = CARTESIAN_POINT ( 'NONE',  ( 4.081241395634245706, 18.69448487464559250, -0.1415844030543617349 ) ) ;
#19028 = DIRECTION ( 'NONE',  ( -0.2490110332224850509, 0.000000000000000000, 0.9685006480810792739 ) ) ;
#19029 = CARTESIAN_POINT ( 'NONE',  ( 46.03750000000000142, -14.84248999999999974, -10.31874999999999964 ) ) ;
#19030 = CARTESIAN_POINT ( 'NONE',  ( 20.92591353227786044, -2.395484007738812871, -13.91390478273180165 ) ) ;
#19031 = CYLINDRICAL_SURFACE ( 'NONE', #8506, 0.7950200000000000600 ) ;
#19032 = AXIS2_PLACEMENT_3D ( 'NONE', #1392, #13255, #8134 ) ;
#19033 = CARTESIAN_POINT ( 'NONE',  ( 11.35066781222083065, 13.35192466491865204, 6.773944610407871991 ) ) ;
#19034 = ORIENTED_EDGE ( 'NONE', *, *, #12642, .F. ) ;
#19035 = AXIS2_PLACEMENT_3D ( 'NONE', #3125, #19807, #19492 ) ;
#19036 = CARTESIAN_POINT ( 'NONE',  ( 12.79472653632228507, -3.968114999999999615, -13.31637763425449883 ) ) ;
#19037 = CARTESIAN_POINT ( 'NONE',  ( 12.04285459910253664, 11.22180268030754213, 0.9169839392688694524 ) ) ;
#19038 = DIRECTION ( 'NONE',  ( 0.000000000000000000, 1.000000000000000000, 0.000000000000000000 ) ) ;
#19039 = ORIENTED_EDGE ( 'NONE', *, *, #18675, .F. ) ;
#19040 = PRODUCT_CONTEXT ( 'NONE', #20604, 'mechanical' ) ;
#19041 = CARTESIAN_POINT ( 'NONE',  ( 30.02465935949302533, -6.754812500000002551, -2.324128137548288731 ) ) ;
#19042 = FACE_BOUND ( 'NONE', #8275, .T. ) ;
#19043 = PRODUCT_DEFINITION_SHAPE ( 'NONE', 'NONE',  #471 ) ;
#19044 = ORIENTED_EDGE ( 'NONE', *, *, #4185, .T. ) ;
#19045 = CARTESIAN_POINT ( 'NONE',  ( 12.01669072522048154, 20.94460807410368020, 3.624609020444634844 ) ) ;
#19046 = CIRCLE ( 'NONE', #15190, 0.5080000000000022276 ) ;
#19047 = CARTESIAN_POINT ( 'NONE',  ( 9.143268736852048661, 21.15296384697220233, 1.757390325529230024 ) ) ;
#19048 = CARTESIAN_POINT ( 'NONE',  ( -0.02560407305274986500, 21.02721105424156178, 4.690030914906221149 ) ) ;
#19049 = DIRECTION ( 'NONE',  ( -0.5087559856598092844, 0.000000000000000000, -0.8609107660235849613 ) ) ;
#19050 = EDGE_CURVE ( 'NONE', #11624, #14525, #46, .T. ) ;
#19051 = DIRECTION ( 'NONE',  ( -0.2490110332224848011, 0.000000000000000000, 0.9685006480810792739 ) ) ;
#19052 = CARTESIAN_POINT ( 'NONE',  ( 13.93302862726156199, 0.5950094174631964661, -16.09203730721210235 ) ) ;
#19053 = FACE_OUTER_BOUND ( 'NONE', #15618, .T. ) ;
#19054 = VECTOR ( 'NONE', #10740, 1000.000000000000114 ) ;
#19055 = ORIENTED_EDGE ( 'NONE', *, *, #21483, .T. ) ;
#19056 = APPLICATION_CONTEXT ( 'automotive_design' ) ;
#19057 = CARTESIAN_POINT ( 'NONE',  ( 8.808541549489559586, 20.20056482616064031, 6.590010215270987182 ) ) ;
#19058 = CARTESIAN_POINT ( 'NONE',  ( 12.25799425556778388, -1.983739999999999393, 0.2069032437451798767 ) ) ;
#19059 = EDGE_LOOP ( 'NONE', ( #19968, #12541, #5366, #7838 ) ) ;
#19060 = CARTESIAN_POINT ( 'NONE',  ( 9.762688185902014482, 11.89947507744004795, -0.1889497053391823445 ) ) ;
#19061 = FACE_OUTER_BOUND ( 'NONE', #3295, .T. ) ;
#19062 = CARTESIAN_POINT ( 'NONE',  ( 12.58831425534056869, 22.00048094112651853, -0.3068354446663246748 ) ) ;
#19063 = AXIS2_PLACEMENT_3D ( 'NONE', #7033, #20505, #13927 ) ;
#19065 = DIRECTION ( 'NONE',  ( 0.000000000000000000, 1.000000000000000000, 0.000000000000000000 ) ) ;
#19064 = CARTESIAN_POINT ( 'NONE',  ( 2.443839657807668431, 20.56225727104456169, 2.139178112839631218 ) ) ;
#19066 = ORIENTED_EDGE ( 'NONE', *, *, #10687, .F. ) ;
#19067 = CARTESIAN_POINT ( 'NONE',  ( 7.531689760312532123, 14.42957034058409604, 8.057596976765562857 ) ) ;
#19068 = VECTOR ( 'NONE', #15337, 1000.000000000000000 ) ;
#19069 = ORIENTED_EDGE ( 'NONE', *, *, #14252, .T. ) ;
#19070 = LINE ( 'NONE', #9345, #3675 ) ;
#19071 = EDGE_CURVE ( 'NONE', #6701, #5934, #3107, .T. ) ;
#19072 = CARTESIAN_POINT ( 'NONE',  ( 0.03263962654255925938, 15.61251617902083844, 0.8683832099246990843 ) ) ;
#19073 = CARTESIAN_POINT ( 'NONE',  ( 19.14286813974102586, -0.2525960963907294965, -14.62579786283977867 ) ) ;
#19074 = ORIENTED_EDGE ( 'NONE', *, *, #19798, .T. ) ;
#19075 = CARTESIAN_POINT ( 'NONE',  ( 53.46798503507454825, 32.54502000000000095, 6.304111036318381878 ) ) ;
#19076 = CARTESIAN_POINT ( 'NONE',  ( 2.077130412032726081, 17.63363686242983519, 0.2456684943282234079 ) ) ;
#19077 = ADVANCED_FACE ( 'NONE', ( #16603 ), #15067, .T. ) ;
#19078 = ADVANCED_FACE ( 'NONE', ( #18466 ), #15395, .T. ) ;
#19079 = AXIS2_PLACEMENT_3D ( 'NONE', #14674, #9223, #4261 ) ;
#19080 = DIRECTION ( 'NONE',  ( 0.000000000000000000, 1.000000000000000000, 0.000000000000000000 ) ) ;
#19081 = VECTOR ( 'NONE', #18703, 1000.000000000000000 ) ;
#19082 = CARTESIAN_POINT ( 'NONE',  ( 39.93069333242032570, 38.88803500000010160, -3.008993689095761148 ) ) ;
#19083 = DIRECTION ( 'NONE',  ( -0.9685006480810790519, 0.000000000000000000, -0.2490110332224857170 ) ) ;
#19084 = ORIENTED_EDGE ( 'NONE', *, *, #7381, .T. ) ;
#19085 = FACE_OUTER_BOUND ( 'NONE', #20271, .T. ) ;
#19086 = DIRECTION ( 'NONE',  ( 0.2490110332224850509, 0.000000000000000000, -0.9685006480810792739 ) ) ;
#19088 = CARTESIAN_POINT ( 'NONE',  ( -15.27766260488554195, 38.49878000000000355, -26.04727837583638461 ) ) ;
#19087 = CARTESIAN_POINT ( 'NONE',  ( 36.73521423675246922, 34.52875999999999834, 2.413462327205186497 ) ) ;
#19089 = VECTOR ( 'NONE', #487, 1000.000000000000114 ) ;
#19090 = ORIENTED_EDGE ( 'NONE', *, *, #17228, .F. ) ;
#19091 = EDGE_LOOP ( 'NONE', ( #20513, #15771, #18340, #16982 ) ) ;
#19092 = AXIS2_PLACEMENT_3D ( 'NONE', #14801, #6367, #18211 ) ;
#19094 = CARTESIAN_POINT ( 'NONE',  ( 34.72145145287101542, 37.11476346399999926, 0.5851394578805096947 ) ) ;
#19093 = CARTESIAN_POINT ( 'NONE',  ( 4.415446871197127976, 20.54185615358932182, 0.3855645798335944896 ) ) ;
#19095 = CIRCLE ( 'NONE', #4631, 2.381250000000001421 ) ;
#19096 = ORIENTED_EDGE ( 'NONE', *, *, #18578, .F. ) ;
#19098 = CARTESIAN_POINT ( 'NONE',  ( 10.49532457957784359, -3.825071637629403387, -16.01826837021063099 ) ) ;
#19097 = CARTESIAN_POINT ( 'NONE',  ( 5.345771735889576881, 12.47140775907805832, 7.152587718021153229 ) ) ;
#19099 = ORIENTED_EDGE ( 'NONE', *, *, #7404, .F. ) ;
#19100 = ORIENTED_EDGE ( 'NONE', *, *, #20903, .F. ) ;
#19101 = EDGE_CURVE ( 'NONE', #6924, #8259, #8869, .T. ) ;
#19102 = CARTESIAN_POINT ( 'NONE',  ( 1.362477653891336793, 13.51601408089542211, 7.762560417787443434 ) ) ;
#19103 = ORIENTED_EDGE ( 'NONE', *, *, #3116, .F. ) ;
#19104 = VECTOR ( 'NONE', #4021, 1000.000000000000000 ) ;
#19105 = VECTOR ( 'NONE', #21738, 1000.000000000000000 ) ;
#19106 = EDGE_CURVE ( 'NONE', #9783, #20277, #18569, .T. ) ;
#19107 = CARTESIAN_POINT ( 'NONE',  ( 31.06384331886062711, 38.48766750000000059, 1.146004012482531476 ) ) ;
#19108 = CARTESIAN_POINT ( 'NONE',  ( 52.44708915697334106, 34.52875999999999834, 4.020247972991190188 ) ) ;
#19109 = DIRECTION ( 'NONE',  ( 0.9724402360367340181, 0.000000000000000000, -0.2331522835762512846 ) ) ;
#19110 = DIRECTION ( 'NONE',  ( 0.9685006480810793850, 0.000000000000000000, 0.2490110332224846623 ) ) ;
#19111 = CARTESIAN_POINT ( 'NONE',  ( 3.241640988598431861, 18.85000704986485687, 8.551504305367847891 ) ) ;
#19112 = VECTOR ( 'NONE', #1759, 1000.000000000000000 ) ;
#19113 = CARTESIAN_POINT ( 'NONE',  ( 19.84534036711146143, -1.573540299197002224, -15.46898262837090243 ) ) ;
#19114 = VERTEX_POINT ( 'NONE', #18669 ) ;
#19115 = CARTESIAN_POINT ( 'NONE',  ( -0.2597389653420326683, 20.42992192302084220, 3.722174571042816460 ) ) ;
#19116 = CARTESIAN_POINT ( 'NONE',  ( 53.10651001381376091, 40.07865999999999929, -16.70269254552787075 ) ) ;
#19117 = CARTESIAN_POINT ( 'NONE',  ( 30.78626241496060700, 2.019535839764540430, -2.552201779827368622 ) ) ;
#19118 = DIRECTION ( 'NONE',  ( -0.9987059298363656357, -0.000000000000000000, -0.05085730733808393328 ) ) ;
#19119 = ORIENTED_EDGE ( 'NONE', *, *, #13924, .T. ) ;
#19120 = EDGE_LOOP ( 'NONE', ( #14595, #12716, #18884, #12143 ) ) ;
#19121 = CARTESIAN_POINT ( 'NONE',  ( 10.93510241507968850, 15.70746112734460986, 7.398426013499326714 ) ) ;
#19122 = DIRECTION ( 'NONE',  ( 0.3928209820863022839, 0.000000000000000000, -0.9196149607486564515 ) ) ;
#19123 = CARTESIAN_POINT ( 'NONE',  ( 11.69641261104832353, 10.74240771329982103, -0.5047199525474890258 ) ) ;
#19124 = VERTEX_POINT ( 'NONE', #21782 ) ;
#19125 = CIRCLE ( 'NONE', #13494, 1.587500000000001688 ) ;
#19126 = VERTEX_POINT ( 'NONE', #16812 ) ;
#19127 = CARTESIAN_POINT ( 'NONE',  ( 46.03750000000000142, 32.54502000000000095, -10.31874999999999964 ) ) ;
#19128 = VECTOR ( 'NONE', #8725, 1000.000000000000000 ) ;
#19129 = VECTOR ( 'NONE', #5546, 1000.000000000000227 ) ;
#19130 = CARTESIAN_POINT ( 'NONE',  ( 7.650701833136086982, 11.68635701119769976, -0.4599083425468352693 ) ) ;
#19131 = CARTESIAN_POINT ( 'NONE',  ( 1.927950833816268084, 16.41909622821189885, -0.03018426488458642726 ) ) ;
#19132 = CARTESIAN_POINT ( 'NONE',  ( 1.670997140563193373, 34.12394749999999988, -22.76294857149378714 ) ) ;
#19133 = ADVANCED_FACE ( 'NONE', ( #1652 ), #8393, .T. ) ;
#19134 = CARTESIAN_POINT ( 'NONE',  ( 5.863121774503869510, 12.63765592565710705, 0.4230228709285713262 ) ) ;
#19135 = EDGE_CURVE ( 'NONE', #12957, #9108, #6860, .T. ) ;
#19136 = AXIS2_PLACEMENT_3D ( 'NONE', #7999, #4897, #9760 ) ;
#19137 = EDGE_CURVE ( 'NONE', #9564, #13936, #4088, .T. ) ;
#19138 = AXIS2_PLACEMENT_3D ( 'NONE', #5632, #330, #553 ) ;
#19139 = CARTESIAN_POINT ( 'NONE',  ( 2.615483950589470474, 19.61703011493782967, 6.888558279248298888 ) ) ;
#19140 = CARTESIAN_POINT ( 'NONE',  ( 17.30373842852263877, 34.52875999999999834, -12.15706637069277107 ) ) ;
#19141 = CARTESIAN_POINT ( 'NONE',  ( 10.13601329052621658, 10.83116634084218077, 0.1401833725585602819 ) ) ;
#19142 = AXIS2_PLACEMENT_3D ( 'NONE', #1252, #15089, #21590 ) ;
#19143 = CARTESIAN_POINT ( 'NONE',  ( 6.707153380113150654, 10.91793053508332001, 4.254858596453126474 ) ) ;
#19144 = DIRECTION ( 'NONE',  ( 0.000000000000000000, 1.000000000000000000, 0.000000000000000000 ) ) ;
#19145 = CARTESIAN_POINT ( 'NONE',  ( 59.55063415577301811, -1.983739999999999837, -22.52230776719629191 ) ) ;
#19146 = CARTESIAN_POINT ( 'NONE',  ( 0.3918216066353466531, 18.57721708583670761, 1.314797039972573689 ) ) ;
#19147 = CARTESIAN_POINT ( 'NONE',  ( 37.51913901087312553, 42.06303499999999929, -14.58057485080488114 ) ) ;
#19148 = CARTESIAN_POINT ( 'NONE',  ( 49.13030338002142372, 0.000000000000000000, -2.154981381712871791 ) ) ;
#19149 = CARTESIAN_POINT ( 'NONE',  ( 11.84053051238870147, 0.2936998923501951686, -16.70720445209922289 ) ) ;
#19150 = CARTESIAN_POINT ( 'NONE',  ( 31.04121718565060206, 34.52875999999999834, -8.720124554639784975 ) ) ;
#19151 = AXIS2_PLACEMENT_3D ( 'NONE', #8106, #21815, #18386 ) ;
#19152 = AXIS2_PLACEMENT_3D ( 'NONE', #10906, #17655, #5919 ) ;
#19153 = LINE ( 'NONE', #5039, #19456 ) ;
#19154 = CARTESIAN_POINT ( 'NONE',  ( 9.826606975627045770, 10.88625345693648150, 0.1783350857751269669 ) ) ;
#19155 = ORIENTED_EDGE ( 'NONE', *, *, #5838, .T. ) ;
#19156 = CARTESIAN_POINT ( 'NONE',  ( 23.63592995296846766, 23.18727947754285879, -3.311609719350443015 ) ) ;
#19157 = CARTESIAN_POINT ( 'NONE',  ( 12.00933040723107403, 11.24147212942736118, 0.7726907669949114599 ) ) ;
#19158 = CARTESIAN_POINT ( 'NONE',  ( 5.363080482404605220, 15.22688935535643573, -2.039950826354700819 ) ) ;
#19159 = CARTESIAN_POINT ( 'NONE',  ( 2.282999857009965439, 20.09148914161242061, 6.315958300496411049 ) ) ;
#19160 = ORIENTED_EDGE ( 'NONE', *, *, #17583, .F. ) ;
#19161 = CONTEXT_DEPENDENT_SHAPE_REPRESENTATION ( #17950, #6678 ) ;
#19162 = DIRECTION ( 'NONE',  ( 0.9964481331860213231, 0.000000000000000000, -0.08420877549337293932 ) ) ;
#19163 = AXIS2_PLACEMENT_3D ( 'NONE', #16580, #5947, #11155 ) ;
#19164 = CARTESIAN_POINT ( 'NONE',  ( 5.468534317627838703, 20.74776807699790027, 3.317767048404099750 ) ) ;
#19165 = EDGE_CURVE ( 'NONE', #8304, #13851, #2885, .T. ) ;
#19166 = DIRECTION ( 'NONE',  ( 0.8558687090795832342, 0.000000000000000000, -0.5171931484643309540 ) ) ;
#19167 = ORIENTED_EDGE ( 'NONE', *, *, #10744, .T. ) ;
#19168 = VECTOR ( 'NONE', #15306, 1000.000000000000227 ) ;
#19169 = CARTESIAN_POINT ( 'NONE',  ( 9.817900122067920066, 21.04886798522784375, 3.383858994149747002 ) ) ;
#19170 = CARTESIAN_POINT ( 'NONE',  ( 4.844186739043601975, 19.02074804359552118, 7.142938902112708988 ) ) ;
#19171 = CARTESIAN_POINT ( 'NONE',  ( 9.040336234276225014, 18.23310434598736052, 6.937167086216335044 ) ) ;
#19172 = CARTESIAN_POINT ( 'NONE',  ( 29.01020070778135818, -1.983739999999999393, -13.85841188422236492 ) ) ;
#19173 = CARTESIAN_POINT ( 'NONE',  ( 19.08799226225449885, -0.6592077476704274464, -14.48249918540156855 ) ) ;
#19174 = CARTESIAN_POINT ( 'NONE',  ( 39.42154620619643879, -5.166360000000000063, -4.343957374020580353 ) ) ;
#19175 = VERTEX_POINT ( 'NONE', #7298 ) ;
#19176 = CARTESIAN_POINT ( 'NONE',  ( 10.63308548515679774, 21.89042938493124169, 0.05754589513367810993 ) ) ;
#19177 = CARTESIAN_POINT ( 'NONE',  ( 52.91086381164393515, 37.11476346399999926, 3.812938856729753301 ) ) ;
#19178 = ORIENTED_EDGE ( 'NONE', *, *, #9791, .F. ) ;
#19179 = CARTESIAN_POINT ( 'NONE',  ( 9.393035566209373854, 17.09556050276089678, -2.811126736337388632 ) ) ;
#19180 = DIRECTION ( 'NONE',  ( 0.08420877549337300871, 0.000000000000000000, 0.9964481331860212121 ) ) ;
#19181 = DIRECTION ( 'NONE',  ( 0.000000000000000000, 1.000000000000000000, 0.000000000000000000 ) ) ;
#19183 = FACE_OUTER_BOUND ( 'NONE', #11215, .T. ) ;
#19182 = CARTESIAN_POINT ( 'NONE',  ( 4.545153868657309637, 11.72601213311298274, 5.605246626590751013 ) ) ;
#19184 = VERTEX_POINT ( 'NONE', #21000 ) ;
#19185 = CARTESIAN_POINT ( 'NONE',  ( 7.176498194401259134, 11.94873204706878056, 6.222147181184805476 ) ) ;
#19186 = CARTESIAN_POINT ( 'NONE',  ( 12.91596452321051558, 13.08893749999999834, 2.799331278665067479 ) ) ;
#19187 = EDGE_CURVE ( 'NONE', #7846, #7070, #5407, .T. ) ;
#19188 = CARTESIAN_POINT ( 'NONE',  ( 39.48015564263409516, -5.405895081254803891, -3.409410579613285197 ) ) ;
#19189 = ORIENTED_EDGE ( 'NONE', *, *, #4405, .F. ) ;
#19190 = CARTESIAN_POINT ( 'NONE',  ( 19.36217743480797893, 0.4374727505662669436, -15.01545013472033396 ) ) ;
#19191 = CARTESIAN_POINT ( 'NONE',  ( 0.06220981948177380788, 14.29877793608298830, 1.344091684615118965 ) ) ;
#19192 = CIRCLE ( 'NONE', #14266, 0.5080000000000013394 ) ;
#19193 = PRODUCT ( 'Handle Pawl Torsion Spring', 'Handle Pawl Torsion Spring', '', ( #20806 ) ) ;
#19194 = CARTESIAN_POINT ( 'NONE',  ( 12.51121735021641612, -6.118460377156197616, -15.53362352737866736 ) ) ;
#19195 = ORIENTED_EDGE ( 'NONE', *, *, #19670, .T. ) ;
#19196 = DIRECTION ( 'NONE',  ( 0.000000000000000000, 1.000000000000000000, 0.000000000000000000 ) ) ;
#19197 = CARTESIAN_POINT ( 'NONE',  ( 13.35516194159795234, 12.73805723869360129, 6.121469047959861243 ) ) ;
#19198 = AXIS2_PLACEMENT_3D ( 'NONE', #5820, #514, #16015 ) ;
#19199 = DIRECTION ( 'NONE',  ( 0.2490110332224846623, 0.000000000000000000, -0.9685006480810793850 ) ) ;
#19200 = CARTESIAN_POINT ( 'NONE',  ( 38.94885947252247860, -7.547248457916676756, -3.956611957470116625 ) ) ;
#19201 = VERTEX_POINT ( 'NONE', #5749 ) ;
#19202 = CARTESIAN_POINT ( 'NONE',  ( 17.30373842852263877, 36.51313500000000545, -12.15706637069277107 ) ) ;
#19203 = LINE ( 'NONE', #630, #4509 ) ;
#19204 = AXIS2_PLACEMENT_3D ( 'NONE', #4445, #12858, #16174 ) ;
#19205 = ORIENTED_EDGE ( 'NONE', *, *, #4095, .F. ) ;
#19207 = CARTESIAN_POINT ( 'NONE',  ( 2.915917464538113180, -1.983739999999999393, -18.72348548116188027 ) ) ;
#19206 = CARTESIAN_POINT ( 'NONE',  ( 2.491886806202981752, 20.82653447492750232, 6.619722005571624379 ) ) ;
#19208 = VERTEX_POINT ( 'NONE', #19116 ) ;
#19209 = CARTESIAN_POINT ( 'NONE',  ( 5.592450108068661940, 15.67876173997583322, 8.758473581429681687 ) ) ;
#19210 = VERTEX_POINT ( 'NONE', #8724 ) ;
#19211 = ADVANCED_FACE ( 'NONE', ( #17471 ), #10829, .T. ) ;
#19212 = ORIENTED_EDGE ( 'NONE', *, *, #20237, .F. ) ;
#19213 = EDGE_CURVE ( 'NONE', #11803, #17975, #8948, .T. ) ;
#19214 = VECTOR ( 'NONE', #4567, 1000.000000000000000 ) ;
#19215 = CARTESIAN_POINT ( 'NONE',  ( 1.292113498908112890, 13.15017386328606186, 7.382771724034875582 ) ) ;
#19216 = ORIENTED_EDGE ( 'NONE', *, *, #360, .F. ) ;
#19217 = CARTESIAN_POINT ( 'NONE',  ( 3.269967501978980451, 13.23265724051127634, 7.157293919752532041 ) ) ;
#19218 = AXIS2_PLACEMENT_3D ( 'NONE', #8043, #14816, #7720 ) ;
#19219 = CARTESIAN_POINT ( 'NONE',  ( -29.36874999999999858, 30.56064500000000095, -3.968750000000000000 ) ) ;
#19220 = LINE ( 'NONE', #1976, #4033 ) ;
#19221 = CARTESIAN_POINT ( 'NONE',  ( 1.405219880766735541, 23.42673279364623085, 8.655316695198486343 ) ) ;
#19222 = CARTESIAN_POINT ( 'NONE',  ( 49.41235866845560309, 0.000000000000000000, -26.78690084448080100 ) ) ;
#19223 = CARTESIAN_POINT ( 'NONE',  ( 2.996463091073017893, 19.66541386574806793, 7.962514975033100129 ) ) ;
#19224 = CARTESIAN_POINT ( 'NONE',  ( 19.99079755883271758, -2.044740353336991223, -15.40828390584228202 ) ) ;
#19225 = VERTEX_POINT ( 'NONE', #14062 ) ;
#19226 = CARTESIAN_POINT ( 'NONE',  ( -0.4304425378944187197, 20.20483442592724188, 3.283658422123586718 ) ) ;
#19227 = AXIS2_PLACEMENT_3D ( 'NONE', #21225, #7745, #16567 ) ;
#19228 = DIRECTION ( 'NONE',  ( -0.000000000000000000, -1.000000000000000000, 0.000000000000000000 ) ) ;
#19229 = CARTESIAN_POINT ( 'NONE',  ( 6.585898268469219552, 1.984375000000000000, 4.694966092919240275 ) ) ;
#19230 = PLANE ( 'NONE',  #67 ) ;
#19231 = ADVANCED_FACE ( 'NONE', ( #3877 ), #10503, .T. ) ;
#19232 = FACE_OUTER_BOUND ( 'NONE', #12673, .T. ) ;
#19233 = VERTEX_POINT ( 'NONE', #5517 ) ;
#19234 = CARTESIAN_POINT ( 'NONE',  ( 5.914053747146598816, 20.37078616557504063, 0.1005632906319847558 ) ) ;
#19236 = LINE ( 'NONE', #17586, #7488 ) ;
#19235 = FACE_OUTER_BOUND ( 'NONE', #20300, .T. ) ;
#19237 = CARTESIAN_POINT ( 'NONE',  ( 13.30192323483472983, 13.36279638818773208, 6.395705296019483121 ) ) ;
#19238 = ORIENTED_EDGE ( 'NONE', *, *, #14997, .F. ) ;
#19239 = AXIS2_PLACEMENT_3D ( 'NONE', #1084, #8154, #18121 ) ;
#19240 = ORIENTED_EDGE ( 'NONE', *, *, #7760, .T. ) ;
#19241 = DIRECTION ( 'NONE',  ( -0.000000000000000000, -1.000000000000000000, 0.000000000000000000 ) ) ;
#19242 = CARTESIAN_POINT ( 'NONE',  ( 7.396207190460517999, 17.87138037546853653, -2.699953620006905197 ) ) ;
#19243 = CARTESIAN_POINT ( 'NONE',  ( 5.397938743089579994, 14.21717427261922673, 7.611741220669421715 ) ) ;
#19244 = LINE ( 'NONE', #15740, #3117 ) ;
#19245 = EDGE_CURVE ( 'NONE', #12825, #9456, #2165, .T. ) ;
#19246 = CARTESIAN_POINT ( 'NONE',  ( 5.639233624224025299, 14.00976992351738559, -0.7654035218331123325 ) ) ;
#19247 = FACE_OUTER_BOUND ( 'NONE', #20552, .T. ) ;
#19248 = EDGE_CURVE ( 'NONE', #723, #10564, #17003, .T. ) ;
#19249 = DIRECTION ( 'NONE',  ( 0.05085730733808139364, 0.000000000000000000, -0.9987059298363658577 ) ) ;
#19250 = CARTESIAN_POINT ( 'NONE',  ( 6.578503335167750876, 20.62467454825192092, -0.2978276507856368327 ) ) ;
#19251 = CIRCLE ( 'NONE', #7255, 0.7950200000000003930 ) ;
#19252 = CARTESIAN_POINT ( 'NONE',  ( -15.39353573898878658, 37.13217763270220217, -10.30107656633069979 ) ) ;
#19253 = CARTESIAN_POINT ( 'NONE',  ( 4.649213468993561804, 20.53916262649988056, 6.851662615090752695 ) ) ;
#19254 = CARTESIAN_POINT ( 'NONE',  ( 70.64340948846358970, 0.000000000000000000, -10.93409647675949969 ) ) ;
#19255 = FACE_OUTER_BOUND ( 'NONE', #12064, .T. ) ;
#19256 = CARTESIAN_POINT ( 'NONE',  ( 1.842148214019495800, 14.88408257588732653, 0.2398186081272557224 ) ) ;
#19257 = CARTESIAN_POINT ( 'NONE',  ( 23.41562500000000213, 32.54502000000000095, 5.159374999999999822 ) ) ;
#19258 = CARTESIAN_POINT ( 'NONE',  ( 26.59062499999999929, 30.16440499999999858, 8.731249999999999289 ) ) ;
#19259 = CARTESIAN_POINT ( 'NONE',  ( 17.48992360529581092, 2.001781804147173549, -15.01608738236844687 ) ) ;
#19260 = EDGE_CURVE ( 'NONE', #13482, #10479, #6760, .T. ) ;
#19261 = ORIENTED_EDGE ( 'NONE', *, *, #6111, .F. ) ;
#19262 = EDGE_CURVE ( 'NONE', #8566, #19617, #19001, .T. ) ;
#19263 = CARTESIAN_POINT ( 'NONE',  ( 59.55063415577301811, 32.54502000000000095, -22.52230776719629191 ) ) ;
#19264 = EDGE_CURVE ( 'NONE', #8553, #16810, #13859, .T. ) ;
#19265 = DIRECTION ( 'NONE',  ( 0.000000000000000000, 1.000000000000000000, 0.000000000000000000 ) ) ;
#19266 = CARTESIAN_POINT ( 'NONE',  ( 9.490334072463598503, 11.65861747434272111, -1.267925462873313425 ) ) ;
#19267 = ORIENTED_EDGE ( 'NONE', *, *, #4646, .F. ) ;
#19268 = DIRECTION ( 'NONE',  ( -0.000000000000000000, -1.000000000000000000, 0.000000000000000000 ) ) ;
#19269 = CARTESIAN_POINT ( 'NONE',  ( 11.64810702638509099, 11.73795319285898131, -0.8004304160343337360 ) ) ;
#19270 = CARTESIAN_POINT ( 'NONE',  ( 5.919258205413525431, 19.60814919271167867, -1.127688298506704045 ) ) ;
#19271 = CARTESIAN_POINT ( 'NONE',  ( 0.05261182704408059324, 23.41816500000000190, 7.316601101023040066 ) ) ;
#19272 = CARTESIAN_POINT ( 'NONE',  ( 3.049654375162700326, 12.59595915030716284, 6.508823439574863201 ) ) ;
#19273 = VERTEX_POINT ( 'NONE', #3985 ) ;
#19274 = CARTESIAN_POINT ( 'NONE',  ( 10.10534066920194185, 34.52875999999999834, -14.00784516691476966 ) ) ;
#19275 = VERTEX_POINT ( 'NONE', #2089 ) ;
#19276 = CARTESIAN_POINT ( 'NONE',  ( 11.70823332671042749, 19.71606648096064163, -2.535146659683900072 ) ) ;
#19277 = CARTESIAN_POINT ( 'NONE',  ( 9.269908071869892296, 16.57988186816537279, 7.309237487032761216 ) ) ;
#19278 = DIRECTION ( 'NONE',  ( 0.000000000000000000, -1.000000000000000000, 0.000000000000000000 ) ) ;
#19279 = LINE ( 'NONE', #15777, #21335 ) ;
#19280 = CARTESIAN_POINT ( 'NONE',  ( 5.130991270212533095, 19.13552603310812117, 7.996869729160946960 ) ) ;
#19281 = EDGE_CURVE ( 'NONE', #3095, #16730, #5630, .T. ) ;
#19282 = CARTESIAN_POINT ( 'NONE',  ( 15.04459320328107630, 1.018023609948645269, -15.74799260762002540 ) ) ;
#19283 = EDGE_CURVE ( 'NONE', #17699, #11223, #9582, .T. ) ;
#19284 = CARTESIAN_POINT ( 'NONE',  ( -0.5435003404963313356, 26.98019749999999917, -25.80650133522849998 ) ) ;
#19285 = ORIENTED_EDGE ( 'NONE', *, *, #4953, .T. ) ;
#19286 = CARTESIAN_POINT ( 'NONE',  ( 7.760365661431780637, 20.10612899863186342, -1.645341292727603655 ) ) ;
#19287 = DIRECTION ( 'NONE',  ( 0.000000000000000000, -1.000000000000000000, -0.000000000000000000 ) ) ;
#19288 = ORIENTED_EDGE ( 'NONE', *, *, #7614, .F. ) ;
#19289 = CARTESIAN_POINT ( 'NONE',  ( 9.306704478242739498, 15.95877063496000581, -2.845665734436647831 ) ) ;
#19290 = CARTESIAN_POINT ( 'NONE',  ( -15.39353573898878658, 34.79968030885680008, -10.30107656633069979 ) ) ;
#19291 = CARTESIAN_POINT ( 'NONE',  ( 0.4932393519182353692, 19.79695343917473949, 6.883184639792627735 ) ) ;
#19293 = DIRECTION ( 'NONE',  ( -0.9685006480810794960, 0.000000000000000000, -0.2490110332224836354 ) ) ;
#19292 = CARTESIAN_POINT ( 'NONE',  ( 2.498689706804295252, 19.49937761787746382, 7.845835893948169826 ) ) ;
#19294 = EDGE_LOOP ( 'NONE', ( #10129, #5753, #9820, #21279, #10040 ) ) ;
#19295 = CARTESIAN_POINT ( 'NONE',  ( 1.663439973261383820, 33.32892749999999893, -22.73355581192510044 ) ) ;
#19296 = CYLINDRICAL_SURFACE ( 'NONE', #13032, 0.7950199999999993938 ) ;
#19297 = EDGE_LOOP ( 'NONE', ( #13253, #1550, #14021, #21305 ) ) ;
#19298 = CARTESIAN_POINT ( 'NONE',  ( 4.520836821130160388, -1.594802499999999013, -5.476444653012091379 ) ) ;
#19299 = CARTESIAN_POINT ( 'NONE',  ( 0.02858491886840053980, 15.02004020798568185, 1.018833874744118129 ) ) ;
#19300 = CARTESIAN_POINT ( 'NONE',  ( 19.10310856060884532, -0.2463609076444987778, -14.44080317216485376 ) ) ;
#19301 = ORIENTED_EDGE ( 'NONE', *, *, #14384, .T. ) ;
#19302 = CARTESIAN_POINT ( 'NONE',  ( 46.03750000000000142, 42.06303499999999929, -10.31874999999999964 ) ) ;
#19303 = CIRCLE ( 'NONE', #5522, 30.16249999999998721 ) ;
#19304 = FACE_OUTER_BOUND ( 'NONE', #1824, .T. ) ;
#19305 = EDGE_CURVE ( 'NONE', #5048, #11296, #18140, .T. ) ;
#19306 = CARTESIAN_POINT ( 'NONE',  ( -15.27766260488554195, -1.983739999999999393, -26.04727837583638461 ) ) ;
#19307 = ORIENTED_EDGE ( 'NONE', *, *, #17237, .T. ) ;
#19308 = CARTESIAN_POINT ( 'NONE',  ( 71.04062499999999147, 30.56064500000000095, -10.31874999999999964 ) ) ;
#19310 = CARTESIAN_POINT ( 'NONE',  ( 54.51779242482700027, 32.54502000000000095, -30.64740209392260084 ) ) ;
#19309 = FACE_OUTER_BOUND ( 'NONE', #18005, .T. ) ;
#19311 = VERTEX_POINT ( 'NONE', #14283 ) ;
#19312 = VERTEX_POINT ( 'NONE', #18783 ) ;
#19313 = CARTESIAN_POINT ( 'NONE',  ( 14.57744845994609584, -8.664519226834075383, -15.14008038430411140 ) ) ;
#19315 = CARTESIAN_POINT ( 'NONE',  ( 17.79723720954694954, 36.51313500000000545, -14.07647485258271303 ) ) ;
#19314 = CARTESIAN_POINT ( 'NONE',  ( 3.618629837795121595, 17.35319764795464792, -1.453827791231713018 ) ) ;
#19316 = ORIENTED_EDGE ( 'NONE', *, *, #2598, .T. ) ;
#19317 = CARTESIAN_POINT ( 'NONE',  ( 4.968297847841906645, 11.40330044108586094, 5.455941518735753171 ) ) ;
#19318 = EDGE_LOOP ( 'NONE', ( #19238, #20805, #3202, #935 ) ) ;
#19319 = CIRCLE ( 'NONE', #15814, 1.190624999999999378 ) ;
#19320 = EDGE_LOOP ( 'NONE', ( #6707, #18946, #11904, #605 ) ) ;
#19321 = ORIENTED_EDGE ( 'NONE', *, *, #3026, .T. ) ;
#19322 = CARTESIAN_POINT ( 'NONE',  ( -22.47451353405102026, 43.41875999999999891, -25.43908013252627853 ) ) ;
#19323 = DIRECTION ( 'NONE',  ( -0.5733392046337749681, 0.8193181045417647912, 0.000000000000000000 ) ) ;
#19324 = CARTESIAN_POINT ( 'NONE',  ( 1.532169971477637782, 34.03012968715594866, -20.71839214105750315 ) ) ;
#19325 = CARTESIAN_POINT ( 'NONE',  ( 2.586256820664998735, 11.26173031269666147, 3.955566897847509811 ) ) ;
#19326 = EDGE_CURVE ( 'NONE', #17848, #13038, #16258, .T. ) ;
#19327 = VECTOR ( 'NONE', #14846, 1000.000000000000000 ) ;
#19328 = VERTEX_POINT ( 'NONE', #1204 ) ;
#19329 = CARTESIAN_POINT ( 'NONE',  ( 7.565709627428113038, 13.41850193825106174, 6.761998452700021645 ) ) ;
#19330 = CARTESIAN_POINT ( 'NONE',  ( 32.52436584422698473, 34.52875999999999834, 1.884807767196291284 ) ) ;
#19331 = CARTESIAN_POINT ( 'NONE',  ( 13.30933468305810585, 22.15284641732971593, 1.973535763860893688 ) ) ;
#19332 = CARTESIAN_POINT ( 'NONE',  ( 29.01020070778135818, 34.52875999999999834, -13.85841188422236492 ) ) ;
#19333 = VERTEX_POINT ( 'NONE', #7947 ) ;
#19334 = VERTEX_POINT ( 'NONE', #9599 ) ;
#19335 = CARTESIAN_POINT ( 'NONE',  ( 12.74873341173676167, 12.98021359793846230, 5.958482511230140943 ) ) ;
#19337 = LINE ( 'NONE', #2761, #411 ) ;
#19336 = CARTESIAN_POINT ( 'NONE',  ( 46.03750000000000142, 36.51313500000000545, -10.31874999999999964 ) ) ;
#19338 = CARTESIAN_POINT ( 'NONE',  ( 12.55110607399917022, 10.63801454700946181, 3.044453194121171880 ) ) ;
#19339 = ORIENTED_EDGE ( 'NONE', *, *, #21306, .T. ) ;
#19340 = ORIENTED_EDGE ( 'NONE', *, *, #21551, .F. ) ;
#19341 = LINE ( 'NONE', #9500, #12759 ) ;
#19342 = CARTESIAN_POINT ( 'NONE',  ( 7.370218150239237431, 12.95355782316449655, -1.762137703980258596 ) ) ;
#19343 = LINE ( 'NONE', #4211, #2376 ) ;
#19344 = DIRECTION ( 'NONE',  ( -0.9685006480810790519, 0.000000000000000000, -0.2490110332224857170 ) ) ;
#19345 = CARTESIAN_POINT ( 'NONE',  ( 6.469343941046106217, 20.06331668064719764, 0.3840982914384075131 ) ) ;
#19346 = CIRCLE ( 'NONE', #9808, 1.983740000000000059 ) ;
#19347 = CARTESIAN_POINT ( 'NONE',  ( 2.222337027708588320, 20.17600262083952956, 5.895190365622971385 ) ) ;
#19348 = CARTESIAN_POINT ( 'NONE',  ( 9.335363283976800375, -1.983739999999999393, -14.20581391854862474 ) ) ;
#19349 = EDGE_CURVE ( 'NONE', #14236, #7630, #17360, .T. ) ;
#19350 = CARTESIAN_POINT ( 'NONE',  ( 9.788131959061814769, 19.28339334790884152, -2.994169572174589788 ) ) ;
#19351 = LINE ( 'NONE', #21777, #19407 ) ;
#19352 = LINE ( 'NONE', #12528, #20232 ) ;
#19353 = LINE ( 'NONE', #4655, #18697 ) ;
#19354 = CARTESIAN_POINT ( 'NONE',  ( 1.769989151042760334, 13.02087111295804256, 0.3933944368290009375 ) ) ;
#19355 = LINE ( 'NONE', #18917, #6810 ) ;
#19356 = EDGE_CURVE ( 'NONE', #10995, #12131, #12074, .T. ) ;
#19357 = EDGE_CURVE ( 'NONE', #5833, #16351, #13150, .T. ) ;
#19358 = EDGE_CURVE ( 'NONE', #11223, #20800, #3595, .T. ) ;
#19359 = LINE ( 'NONE', #15752, #8222 ) ;
#19360 = CARTESIAN_POINT ( 'NONE',  ( 3.801506843055717511, 17.18874207142271970, -0.6811624414094943347 ) ) ;
#19361 = CARTESIAN_POINT ( 'NONE',  ( 50.52547294529469468, 38.88803500000000213, -18.64987929725020521 ) ) ;
#19362 = LINE ( 'NONE', #2570, #10662 ) ;
#19363 = CARTESIAN_POINT ( 'NONE',  ( 20.94506505885473757, -2.696405856112658928, -13.89795473303651008 ) ) ;
#19364 = ORIENTED_EDGE ( 'NONE', *, *, #17833, .T. ) ;
#19365 = CARTESIAN_POINT ( 'NONE',  ( 53.46798503507454825, 32.54502000000000095, 6.304111036318381878 ) ) ;
#19366 = VECTOR ( 'NONE', #16816, 1000.000000000000000 ) ;
#19367 = CARTESIAN_POINT ( 'NONE',  ( 9.841056877679053017, 10.86540522446826174, 0.2393104589039902752 ) ) ;
#19368 = EDGE_LOOP ( 'NONE', ( #1860, #428, #4929, #15498 ) ) ;
#19369 = CARTESIAN_POINT ( 'NONE',  ( 54.11611804786240043, 0.000000000000000000, -30.58983753981140197 ) ) ;
#19370 = CARTESIAN_POINT ( 'NONE',  ( 5.681085220776317612, 12.17129757418337199, -0.2378145488336220192 ) ) ;
#19371 = DIRECTION ( 'NONE',  ( 0.05085730733808139364, 0.000000000000000000, -0.9987059298363658577 ) ) ;
#19372 = ORIENTED_EDGE ( 'NONE', *, *, #14369, .F. ) ;
#19373 = CONTEXT_DEPENDENT_SHAPE_REPRESENTATION ( #17530, #1731 ) ;
#19374 = DIRECTION ( 'NONE',  ( 0.000000000000000000, 1.000000000000000000, 0.000000000000000000 ) ) ;
#19375 = CARTESIAN_POINT ( 'NONE',  ( 5.391733748237763635, 20.73460212580145878, 3.114551668807497897 ) ) ;
#19376 = CARTESIAN_POINT ( 'NONE',  ( -7.545238043312568088, 34.12394749999999988, -33.79351368943453338 ) ) ;
#19377 = EDGE_CURVE ( 'NONE', #19979, #7768, #14381, .T. ) ;
#19378 = PRODUCT_DEFINITION ( 'UNKNOWN', '', #1706, #7457 ) ;
#19379 = VECTOR ( 'NONE', #19762, 1000.000000000000000 ) ;
#19380 = ORIENTED_EDGE ( 'NONE', *, *, #3696, .F. ) ;
#19381 = CARTESIAN_POINT ( 'NONE',  ( 10.85750912504734522, 19.10987469415690043, 6.066339372520253015 ) ) ;
#19382 = CARTESIAN_POINT ( 'NONE',  ( 9.931220000398274905, 11.51518149844540240, 0.4432291548185011698 ) ) ;
#19383 = FACE_OUTER_BOUND ( 'NONE', #10068, .T. ) ;
#19384 = ADVANCED_FACE ( 'NONE', ( #14717 ), #14610, .T. ) ;
#19385 = EDGE_CURVE ( 'NONE', #6167, #4861, #21207, .T. ) ;
#19386 = CARTESIAN_POINT ( 'NONE',  ( 53.77854886916050958, -7.114547009363026753, -15.86998015261754880 ) ) ;
#19387 = AXIS2_PLACEMENT_3D ( 'NONE', #14214, #10769, #19483 ) ;
#19388 = LINE ( 'NONE', #2263, #16957 ) ;
#19389 = ORIENTED_EDGE ( 'NONE', *, *, #2643, .T. ) ;
#19390 = ORIENTED_EDGE ( 'NONE', *, *, #12516, .T. ) ;
#19391 = CARTESIAN_POINT ( 'NONE',  ( 10.51466052783852234, 20.82419441543289906, -0.1522035372867676650 ) ) ;
#19392 = CARTESIAN_POINT ( 'NONE',  ( 1.318808768746996929, 17.31501546851630025, 8.734854497731600276 ) ) ;
#19394 = CARTESIAN_POINT ( 'NONE',  ( -12.30312499606204035, 30.56080375000000160, 10.71562494918373964 ) ) ;
#19393 = CARTESIAN_POINT ( 'NONE',  ( 3.029311592522686780, 13.36420590592894264, 8.039591749172359414 ) ) ;
#19395 = VERTEX_POINT ( 'NONE', #9487 ) ;
#19396 = DIRECTION ( 'NONE',  ( 0.000000000000000000, 1.000000000000000000, 0.000000000000000000 ) ) ;
#19397 = CARTESIAN_POINT ( 'NONE',  ( 12.57635667311951622, 34.52875999999999834, 1.354834321244424267 ) ) ;
#19398 = ORIENTED_EDGE ( 'NONE', *, *, #19533, .T. ) ;
#19399 = CIRCLE ( 'NONE', #13788, 0.5079999999999995630 ) ;
#19400 = CARTESIAN_POINT ( 'NONE',  ( 5.447351731530780228, 32.54502000000000095, 0.8930339070797439494 ) ) ;
#19401 = EDGE_CURVE ( 'NONE', #12232, #13358, #19556, .T. ) ;
#19402 = ADVANCED_FACE ( 'NONE', ( #21426 ), #13052, .F. ) ;
#19403 = ADVANCED_FACE ( 'NONE', ( #4633 ), #12800, .T. ) ;
#19404 = CARTESIAN_POINT ( 'NONE',  ( 19.73605314530132304, -0.8007017946179174617, -16.01579480532253186 ) ) ;
#19405 = ORIENTED_EDGE ( 'NONE', *, *, #5282, .F. ) ;
#19406 = DIRECTION ( 'NONE',  ( -0.8943161143440100380, 0.000000000000000000, -0.4474356798743607255 ) ) ;
#19407 = VECTOR ( 'NONE', #8389, 1000.000000000000000 ) ;
#19408 = LINE ( 'NONE', #19306, #1314 ) ;
#19409 = ORIENTED_EDGE ( 'NONE', *, *, #2108, .T. ) ;
#19410 = CIRCLE ( 'NONE', #16275, 30.16249999999999076 ) ;
#19411 = FACE_OUTER_BOUND ( 'NONE', #21660, .T. ) ;
#19412 = AXIS2_PLACEMENT_3D ( 'NONE', #4922, #11563, #7919 ) ;
#19414 = LINE ( 'NONE', #5829, #8376 ) ;
#19413 = DIRECTION ( 'NONE',  ( -0.2490110332224850231, 0.000000000000000000, 0.9685006480810791629 ) ) ;
#19415 = ORIENTED_EDGE ( 'NONE', *, *, #16529, .T. ) ;
#19416 = VERTEX_POINT ( 'NONE', #19330 ) ;
#19417 = CARTESIAN_POINT ( 'NONE',  ( 20.04694561498230598, 0.5575515236321860746, -14.19813339123195561 ) ) ;
#19419 = DIRECTION ( 'NONE',  ( -0.2490110332224846346, 0.000000000000000000, 0.9685006480810792739 ) ) ;
#19418 = CARTESIAN_POINT ( 'NONE',  ( 1.614128406362234980, 17.33698837102782520, 9.606669273329499603 ) ) ;
#19420 = ORIENTED_EDGE ( 'NONE', *, *, #20673, .T. ) ;
#19421 = CARTESIAN_POINT ( 'NONE',  ( 3.662491624849550931, 13.06014951857161321, -0.2875058916943667442 ) ) ;
#19422 = ORIENTED_EDGE ( 'NONE', *, *, #12703, .F. ) ;
#19423 = VERTEX_POINT ( 'NONE', #16149 ) ;
#19424 = CARTESIAN_POINT ( 'NONE',  ( 1.458148681563614879, 14.39063534605306671, 8.374873237808131421 ) ) ;
#19425 = EDGE_CURVE ( 'NONE', #15199, #1402, #18126, .T. ) ;
#19426 = ORIENTED_EDGE ( 'NONE', *, *, #8325, .T. ) ;
#19427 = AXIS2_PLACEMENT_3D ( 'NONE', #2458, #8974, #10858 ) ;
#19428 = AXIS2_PLACEMENT_3D ( 'NONE', #7675, #12779, #19502 ) ;
#19429 = CYLINDRICAL_SURFACE ( 'NONE', #778, 0.5953125000000005773 ) ;
#19430 = CYLINDRICAL_SURFACE ( 'NONE', #2630, 1.785937499999999512 ) ;
#19431 = AXIS2_PLACEMENT_3D ( 'NONE', #4949, #10370, #11817 ) ;
#19432 = CARTESIAN_POINT ( 'NONE',  ( 1.445847263472733291, -1.594802499999999013, -6.267054683493481271 ) ) ;
#19433 = CYLINDRICAL_SURFACE ( 'NONE', #17484, 0.7950200000000000600 ) ;
#19434 = CARTESIAN_POINT ( 'NONE',  ( 2.135935944106437390, 11.82688626209604621, 1.990821043935844026 ) ) ;
#19435 = VERTEX_POINT ( 'NONE', #2652 ) ;
#19436 = CIRCLE ( 'NONE', #17686, 4.365625000000000533 ) ;
#19437 = CARTESIAN_POINT ( 'NONE',  ( 39.47397446732132664, 38.88803500000000213, 2.793231391354656701 ) ) ;
#19438 = DIRECTION ( 'NONE',  ( 0.000000000000000000, 1.000000000000000000, 0.000000000000000000 ) ) ;
#19439 = CYLINDRICAL_SURFACE ( 'NONE', #1139, 3.175000000000000711 ) ;
#19440 = CARTESIAN_POINT ( 'NONE',  ( -17.46249999999999858, 30.56064500000000095, 0.000000000000000000 ) ) ;
#19441 = ORIENTED_EDGE ( 'NONE', *, *, #14796, .T. ) ;
#19442 = EDGE_LOOP ( 'NONE', ( #12929, #6588, #16440, #16463 ) ) ;
#19443 = CARTESIAN_POINT ( 'NONE',  ( 7.052001307456389867, 12.88806360044558197, -1.228466916830508682 ) ) ;
#19445 = CARTESIAN_POINT ( 'NONE',  ( 30.78626241496060700, 30.50833916023545811, -2.552201779827368622 ) ) ;
#19444 = CARTESIAN_POINT ( 'NONE',  ( -17.46249999999999858, 33.73373999999999739, 0.000000000000000000 ) ) ;
#19446 = CARTESIAN_POINT ( 'NONE',  ( 13.21799010538730812, 12.70407506772013129, 5.966476990678911463 ) ) ;
#19447 = ORIENTED_EDGE ( 'NONE', *, *, #19488, .F. ) ;
#19448 = AXIS2_PLACEMENT_3D ( 'NONE', #19150, #2351, #7232 ) ;
#19449 = VERTEX_POINT ( 'NONE', #2984 ) ;
#19450 = CARTESIAN_POINT ( 'NONE',  ( 17.87574706213523612, -1.983739999999999393, -11.18912023382283571 ) ) ;
#19451 = CARTESIAN_POINT ( 'NONE',  ( 7.563764764072376856, 11.98948496040201306, -0.8495171220973293247 ) ) ;
#19452 = CARTESIAN_POINT ( 'NONE',  ( 3.482904747837870740, 20.64447347884702211, 3.584108899128696901 ) ) ;
#19453 = CARTESIAN_POINT ( 'NONE',  ( 7.828815060326342667, 20.77749002548769042, 3.972184785381453587 ) ) ;
#19454 = COLOUR_RGB ( '', 0.31764706, 0.68627451, 0.89019608) ;
#19455 = EDGE_CURVE ( 'NONE', #15606, #19114, #17688, .T. ) ;
#19456 = VECTOR ( 'NONE', #14093, 1000.000000000000227 ) ;
#19457 = CARTESIAN_POINT ( 'NONE',  ( 2.488984304238356593, 19.83350231766241478, 6.572627150490618853 ) ) ;
#19458 = CIRCLE ( 'NONE', #17299, 16.66874999999998508 ) ;
#19459 = DIRECTION ( 'NONE',  ( -0.9579671649362032637, 0.000000000000000000, 0.2868778675745012885 ) ) ;
#19460 = AXIS2_PLACEMENT_3D ( 'NONE', #2206, #551, #15608 ) ;
#19461 = CARTESIAN_POINT ( 'NONE',  ( 14.31159658034589555, 21.56570388316688280, 3.562700818068579522 ) ) ;
#19462 = CARTESIAN_POINT ( 'NONE',  ( 52.91474337680157447, -7.548011381845581624, -16.50491988134626808 ) ) ;
#19463 = LINE ( 'NONE', #10520, #16392 ) ;
#19464 = DIRECTION ( 'NONE',  ( 0.1060008583745224581, 0.000000000000000000, 0.9943660382494288186 ) ) ;
#19465 = CARTESIAN_POINT ( 'NONE',  ( 4.991296504249822519, 11.34913591283086021, 5.626762266647114430 ) ) ;
#19466 = CARTESIAN_POINT ( 'NONE',  ( 1.606218844064036144, 13.47661576675192663, 8.724755388575742288 ) ) ;
#19467 = LINE ( 'NONE', #19145, #17044 ) ;
#19468 = CARTESIAN_POINT ( 'NONE',  ( 1.290330672387997035, 20.33382539468342287, 3.526104413675141380 ) ) ;
#19469 = DIRECTION ( 'NONE',  ( -0.3542738219355860418, 0.000000000000000000, -0.9351417320872557060 ) ) ;
#19470 = DIRECTION ( 'NONE',  ( -0.7421532822901579785, -0.000000000000000000, 0.6702301885068630005 ) ) ;
#19471 = CARTESIAN_POINT ( 'NONE',  ( 19.19346778367484774, -7.066212543700896020, -14.17012739972722279 ) ) ;
#19472 = ORIENTED_EDGE ( 'NONE', *, *, #19953, .T. ) ;
#19473 = CYLINDRICAL_SURFACE ( 'NONE', #5315, 0.7950200000000005041 ) ;
#19474 = VECTOR ( 'NONE', #10859, 1000.000000000000000 ) ;
#19475 = AXIS2_PLACEMENT_3D ( 'NONE', #2547, #16374, #7628 ) ;
#19476 = CARTESIAN_POINT ( 'NONE',  ( 10.08697080318449579, 10.61613734897275130, 1.270570921979556456 ) ) ;
#19477 = ORIENTED_EDGE ( 'NONE', *, *, #9369, .T. ) ;
#19478 = CARTESIAN_POINT ( 'NONE',  ( 28.63992156299379843, 1.561888874053700027, 10.67040950666179988 ) ) ;
#19479 = AXIS2_PLACEMENT_3D ( 'NONE', #10474, #20629, #9029 ) ;
#19480 = CARTESIAN_POINT ( 'NONE',  ( 12.46191723504852433, 21.05992202225752052, -0.6087379413794911098 ) ) ;
#19481 = CARTESIAN_POINT ( 'NONE',  ( 5.508984985521168554, 17.56310428172361782, -2.032606368940984343 ) ) ;
#19482 = AXIS2_PLACEMENT_3D ( 'NONE', #21784, #3122, #111 ) ;
#19483 = DIRECTION ( 'NONE',  ( -0.9822019212503902974, 0.000000000000000000, 0.1878280753562734662 ) ) ;
#19484 = CARTESIAN_POINT ( 'NONE',  ( 0.1070098978122437372, 13.13938098413696132, 2.205990570212618351 ) ) ;
#19485 = ORIENTED_EDGE ( 'NONE', *, *, #18290, .F. ) ;
#19486 =( LENGTH_UNIT ( ) NAMED_UNIT ( * ) SI_UNIT ( .MILLI., .METRE. ) );
#19487 = EDGE_CURVE ( 'NONE', #2577, #3111, #9272, .T. ) ;
#19488 = EDGE_CURVE ( 'NONE', #17560, #3364, #15630, .T. ) ;
#19489 = FACE_OUTER_BOUND ( 'NONE', #3163, .T. ) ;
#19490 = VECTOR ( 'NONE', #11253, 1000.000000000000000 ) ;
#19491 = AXIS2_PLACEMENT_3D ( 'NONE', #20295, #13478, #15043 ) ;
#19492 = DIRECTION ( 'NONE',  ( -0.9724402360367336851, 0.000000000000000000, 0.2331522835762537549 ) ) ;
#19493 = ORIENTED_EDGE ( 'NONE', *, *, #6160, .T. ) ;
#19494 = CARTESIAN_POINT ( 'NONE',  ( 9.943729142003926214, 18.95229069147438139, -2.474586121992937926 ) ) ;
#19495 = CARTESIAN_POINT ( 'NONE',  ( 5.351158161824543846, 16.10253209244224593, 8.037206358779434012 ) ) ;
#19496 = CARTESIAN_POINT ( 'NONE',  ( 29.45491884992628329, -3.968114999999999615, -15.58809351040512325 ) ) ;
#19497 = AXIS2_PLACEMENT_3D ( 'NONE', #3310, #11914, #20082 ) ;
#19498 = AXIS2_PLACEMENT_3D ( 'NONE', #14491, #19657, #2868 ) ;
#19499 = CARTESIAN_POINT ( 'NONE',  ( 53.91018755822011599, -6.683201455308112493, -15.68072631912343518 ) ) ;
#19500 = DIRECTION ( 'NONE',  ( 0.2490110332224850509, 0.000000000000000000, -0.9685006480810792739 ) ) ;
#19501 = CARTESIAN_POINT ( 'NONE',  ( 3.930212692675568498, 21.29697021551619329, 4.866220384958813483 ) ) ;
#19502 = DIRECTION ( 'NONE',  ( 1.000000000000000000, 0.000000000000000000, 0.000000000000000000 ) ) ;
#19503 = ORIENTED_EDGE ( 'NONE', *, *, #7732, .F. ) ;
#19504 = LINE ( 'NONE', #12145, #12445 ) ;
#19505 = EDGE_CURVE ( 'NONE', #11144, #3974, #11030, .T. ) ;
#19506 = CARTESIAN_POINT ( 'NONE',  ( 10.50091842137632270, -3.824863312786503045, -16.03413138725077403 ) ) ;
#19507 = DIRECTION ( 'NONE',  ( 0.000000000000000000, 1.000000000000000000, 0.000000000000000000 ) ) ;
#19508 = ORIENTED_EDGE ( 'NONE', *, *, #17190, .F. ) ;
#19509 = CARTESIAN_POINT ( 'NONE',  ( 10.29536085631526454, 20.49447628526758436, -0.7298637714113751507 ) ) ;
#19510 = DIRECTION ( 'NONE',  ( 0.000000000000000000, -1.000000000000000000, 0.000000000000000000 ) ) ;
#19511 = CARTESIAN_POINT ( 'NONE',  ( 1.417191649792139296, 16.55315478993970402, 8.850408389496440265 ) ) ;
#19512 = CARTESIAN_POINT ( 'NONE',  ( 14.13241029341496358, -8.473400452264066018, -16.35006988243831927 ) ) ;
#19514 = CARTESIAN_POINT ( 'NONE',  ( 14.25617145423489696, -1.983739999999999393, -15.80779474975094168 ) ) ;
#19513 = CARTESIAN_POINT ( 'NONE',  ( 2.002672932925127824, 20.46094657096126213, 6.584029723752546026 ) ) ;
#19515 = ORIENTED_EDGE ( 'NONE', *, *, #1905, .F. ) ;
#19516 =( LENGTH_UNIT ( ) NAMED_UNIT ( * ) SI_UNIT ( .MILLI., .METRE. ) );
#19517 = CARTESIAN_POINT ( 'NONE',  ( 9.275488759993784527, 40.07707250000000698, -20.77642327197297689 ) ) ;
#19518 = VECTOR ( 'NONE', #11328, 1000.000000000000227 ) ;
#19519 = CARTESIAN_POINT ( 'NONE',  ( 1.719806708599410427, 8.992310301660250360, 8.718447211008458098 ) ) ;
#19520 = ORIENTED_EDGE ( 'NONE', *, *, #237, .T. ) ;
#19521 = VECTOR ( 'NONE', #14383, 1000.000000000000000 ) ;
#19522 = EDGE_CURVE ( 'NONE', #7142, #4736, #2905, .T. ) ;
#19523 = DIRECTION ( 'NONE',  ( -0.8609107660235850723, 0.000000000000000000, 0.5087559856598092844 ) ) ;
#19524 = CARTESIAN_POINT ( 'NONE',  ( 19.54280466309461062, -0.8724958927937114250, -15.72700954820671626 ) ) ;
#19525 = EDGE_LOOP ( 'NONE', ( #1838, #11258, #17204, #14682 ) ) ;
#19526 = CARTESIAN_POINT ( 'NONE',  ( 5.655606339218213208, 17.24330370537085955, -1.409341170596322801 ) ) ;
#19527 = AXIS2_PLACEMENT_3D ( 'NONE', #5975, #4338, #17834 ) ;
#19528 = EDGE_CURVE ( 'NONE', #11564, #20988, #14571, .T. ) ;
#19529 = DIRECTION ( 'NONE',  ( 0.9964481331860213231, 0.000000000000000000, -0.08420877549337293932 ) ) ;
#19530 = VECTOR ( 'NONE', #13212, 1000.000000000000000 ) ;
#19531 = VERTEX_POINT ( 'NONE', #15042 ) ;
#19532 = CYLINDRICAL_SURFACE ( 'NONE', #7188, 0.3962400000000000366 ) ;
#19533 = EDGE_CURVE ( 'NONE', #10280, #7768, #9924, .T. ) ;
#19535 = CARTESIAN_POINT ( 'NONE',  ( -15.71080452296940599, -14.84248999999999974, -10.47737680862620380 ) ) ;
#19534 = LINE ( 'NONE', #11135, #5243 ) ;
#19536 = VERTEX_POINT ( 'NONE', #15255 ) ;
#19537 = EDGE_CURVE ( 'NONE', #8141, #9016, #3249, .T. ) ;
#19538 = ORIENTED_EDGE ( 'NONE', *, *, #8176, .F. ) ;
#19539 = EDGE_CURVE ( 'NONE', #8727, #20432, #15993, .T. ) ;
#19540 = CARTESIAN_POINT ( 'NONE',  ( 21.03094872803853121, -1.172420608524037178, -15.10904117410172276 ) ) ;
#19542 = CARTESIAN_POINT ( 'NONE',  ( 22.22454659879084460, 34.52875999999999834, -13.75904720189594244 ) ) ;
#19541 = CARTESIAN_POINT ( 'NONE',  ( 6.291852177003497637, 10.85576871210978211, 2.343863137984593781 ) ) ;
#19543 = ORIENTED_EDGE ( 'NONE', *, *, #20692, .F. ) ;
#19544 = CARTESIAN_POINT ( 'NONE',  ( 3.973159551739567696, 19.20098565268092727, -0.6330842699365994974 ) ) ;
#19545 = VERTEX_POINT ( 'NONE', #10141 ) ;
#19546 = ORIENTED_EDGE ( 'NONE', *, *, #15072, .F. ) ;
#19547 = AXIS2_PLACEMENT_3D ( 'NONE', #18801, #20902, #19017 ) ;
#19548 = ORIENTED_EDGE ( 'NONE', *, *, #20068, .F. ) ;
#19549 = PLANE ( 'NONE',  #1822 ) ;
#19550 = AXIS2_PLACEMENT_3D ( 'NONE', #16595, #8496, #11724 ) ;
#19551 = CARTESIAN_POINT ( 'NONE',  ( 38.96848998618624904, -5.166360000000000063, -3.934807454472129429 ) ) ;
#19552 = CARTESIAN_POINT ( 'NONE',  ( 14.93145837000203358, 15.36419388438619826, -20.01065317369261365 ) ) ;
#19553 = DIRECTION ( 'NONE',  ( -0.9685006480810790519, 0.000000000000000000, -0.2490110332224857170 ) ) ;
#19554 = CARTESIAN_POINT ( 'NONE',  ( 3.518930018599623288, 13.18938088783941787, 8.144277403441783747 ) ) ;
#19555 = ORIENTED_EDGE ( 'NONE', *, *, #20284, .F. ) ;
#19556 = LINE ( 'NONE', #2754, #14226 ) ;
#19557 = DIRECTION ( 'NONE',  ( -0.2868778675745011220, 0.000000000000000000, -0.9579671649362034858 ) ) ;
#19558 = DIRECTION ( 'NONE',  ( -0.6702301885068638887, 0.000000000000000000, -0.7421532822901570903 ) ) ;
#19559 = CYLINDRICAL_SURFACE ( 'NONE', #10559, 3.175000000000000711 ) ;
#19560 = ORIENTED_EDGE ( 'NONE', *, *, #498, .F. ) ;
#19561 = EDGE_CURVE ( 'NONE', #14476, #12395, #81, .T. ) ;
#19562 = ORIENTED_EDGE ( 'NONE', *, *, #14720, .F. ) ;
#19563 = CARTESIAN_POINT ( 'NONE',  ( 10.93405359717582215, 14.00597049205862277, 6.551351406591241933 ) ) ;
#19565 = FACE_BOUND ( 'NONE', #15675, .T. ) ;
#19564 = CARTESIAN_POINT ( 'NONE',  ( 46.03750000000000142, 30.56064500000000095, -10.31874999999999964 ) ) ;
#19566 = AXIS2_PLACEMENT_3D ( 'NONE', #14735, #4766, #9727 ) ;
#19567 = CARTESIAN_POINT ( 'NONE',  ( 11.71072533466843346, 20.55886875348996412, -2.691199719323197126 ) ) ;
#19568 = ORIENTED_EDGE ( 'NONE', *, *, #9263, .T. ) ;
#19569 = EDGE_LOOP ( 'NONE', ( #15124, #1274, #1961, #11266 ) ) ;
#19570 = DIRECTION ( 'NONE',  ( -0.5171931484643297328, 0.000000000000000000, -0.8558687090795841224 ) ) ;
#19571 = CARTESIAN_POINT ( 'NONE',  ( 7.433331065033467411, 18.10929869608010634, -2.625636931304927479 ) ) ;
#19572 = LINE ( 'NONE', #12233, #2041 ) ;
#19573 = CARTESIAN_POINT ( 'NONE',  ( 8.983827027755273420, 18.20566418143656406, 6.849687620904892249 ) ) ;
#19574 = AXIS2_PLACEMENT_3D ( 'NONE', #11372, #9264, #4305 ) ;
#19575 = CARTESIAN_POINT ( 'NONE',  ( 6.680730399758177285, 11.81714183159373199, 4.112448148044469676 ) ) ;
#19576 = DIRECTION ( 'NONE',  ( -0.9964481331860212121, 0.000000000000000000, 0.08420877549337336954 ) ) ;
#19577 = CARTESIAN_POINT ( 'NONE',  ( 7.292079158261280725, 14.37945976953094629, -2.683365525959949593 ) ) ;
#19578 = CARTESIAN_POINT ( 'NONE',  ( 13.70405149357018004, 21.54752288430403695, 1.766493360091446085 ) ) ;
#19579 = DIRECTION ( 'NONE',  ( 0.5222415575336524229, 0.000000000000000000, 0.8527976052879281399 ) ) ;
#19580 = CARTESIAN_POINT ( 'NONE',  ( 3.374943536863300508, 18.28257875309041935, 8.941416396130453137 ) ) ;
#19581 = CARTESIAN_POINT ( 'NONE',  ( 1.456944856587381709, 12.62211961469936128, 7.963006803835855685 ) ) ;
#19582 = CARTESIAN_POINT ( 'NONE',  ( 34.38097451710952868, 0.000000000000000000, 0.2081255904771098786 ) ) ;
#19583 = CARTESIAN_POINT ( 'NONE',  ( 2.925846556779251095, 19.21529397045534182, 7.410183071057827142 ) ) ;
#19584 = CARTESIAN_POINT ( 'NONE',  ( 42.94469661997857912, 42.06303499999999929, -18.48251861828712705 ) ) ;
#19585 = DIRECTION ( 'NONE',  ( 0.000000000000000000, -1.000000000000000000, 0.000000000000000000 ) ) ;
#19586 = CARTESIAN_POINT ( 'NONE',  ( 15.14187524152246844, -8.405880411091629867, -15.04820586386156478 ) ) ;
#19587 = ORIENTED_EDGE ( 'NONE', *, *, #11806, .T. ) ;
#19588 = CARTESIAN_POINT ( 'NONE',  ( -46.55773479047372376, 43.41875999999999891, -7.870535429687039120 ) ) ;
#19589 = ADVANCED_FACE ( 'NONE', ( #16790 ), #6833, .T. ) ;
#19590 = CARTESIAN_POINT ( 'NONE',  ( 9.906809305938214294, 20.59416953720186783, -1.845156594728350141 ) ) ;
#19591 = VERTEX_POINT ( 'NONE', #3513 ) ;
#19592 = CARTESIAN_POINT ( 'NONE',  ( 27.93207353965470574, 34.52875999999999834, -8.388685343514779902 ) ) ;
#19593 = CARTESIAN_POINT ( 'NONE',  ( 11.75807948570318295, 19.66724708567648605, -2.440222580272270569 ) ) ;
#19594 = CARTESIAN_POINT ( 'NONE',  ( 5.761094208437596897, 19.00053386114307230, -1.506891469455103438 ) ) ;
#19595 = CARTESIAN_POINT ( 'NONE',  ( -17.46249999999999858, 32.54502000000000095, 0.000000000000000000 ) ) ;
#19596 = CARTESIAN_POINT ( 'NONE',  ( 3.739208544156527925, 17.18772947144893948, -0.6574115393716641886 ) ) ;
#19597 = EDGE_LOOP ( 'NONE', ( #7399, #10679, #12364, #12701, #20745, #5169 ) ) ;
#19598 = LINE ( 'NONE', #4464, #709 ) ;
#19599 = LINE ( 'NONE', #4357, #147 ) ;
#19600 = CIRCLE ( 'NONE', #1944, 9.525000000000002132 ) ;
#19601 = CARTESIAN_POINT ( 'NONE',  ( 9.243363897212034885, 12.11223639541018215, 5.050083142846552242 ) ) ;
#19602 = CARTESIAN_POINT ( 'NONE',  ( 29.98909767165928386, -5.959792500000001603, -5.214162619065493054 ) ) ;
#19603 = CARTESIAN_POINT ( 'NONE',  ( -3.845402119898529758, 3.961447500000001565, -31.39393985263922460 ) ) ;
#19604 = CARTESIAN_POINT ( 'NONE',  ( 29.31223750860709742, 29.71825598581263961, -5.011466527456265752 ) ) ;
#19605 = PLANE ( 'NONE',  #11031 ) ;
#19606 = DIRECTION ( 'NONE',  ( 0.08420877549337300871, 0.000000000000000000, 0.9964481331860212121 ) ) ;
#19607 = EDGE_CURVE ( 'NONE', #1499, #367, #6610, .T. ) ;
#19608 = VERTEX_POINT ( 'NONE', #18230 ) ;
#19609 = LINE ( 'NONE', #13326, #7851 ) ;
#19610 = DIRECTION ( 'NONE',  ( 0.000000000000000000, 1.000000000000000000, 0.000000000000000000 ) ) ;
#19611 = AXIS2_PLACEMENT_3D ( 'NONE', #20737, #17210, #5594 ) ;
#19612 = ORIENTED_EDGE ( 'NONE', *, *, #212, .F. ) ;
#19613 = CARTESIAN_POINT ( 'NONE',  ( 10.19629082482998150, 20.30350291925140382, -0.9866510706609600279 ) ) ;
#19614 = CARTESIAN_POINT ( 'NONE',  ( 1.082545292382026458, 18.42541199074858227, 8.282403339363888506 ) ) ;
#19615 = CARTESIAN_POINT ( 'NONE',  ( 20.03229091909386739, 0.5637714581750892240, -14.11072859660528955 ) ) ;
#19616 = DIRECTION ( 'NONE',  ( -0.6287118719681975554, 0.000000000000000000, -0.7776383362760898033 ) ) ;
#19617 = VERTEX_POINT ( 'NONE', #20294 ) ;
#19618 = CARTESIAN_POINT ( 'NONE',  ( 41.45112526417833010, 32.54502000000000095, 7.778260066349530710 ) ) ;
#19619 = DIRECTION ( 'NONE',  ( -0.2868778675745011220, 0.000000000000000000, -0.9579671649362034858 ) ) ;
#19620 = ORIENTED_EDGE ( 'NONE', *, *, #137, .T. ) ;
#19621 = DIRECTION ( 'NONE',  ( -0.9579671649362032637, 0.000000000000000000, 0.2868778675745010664 ) ) ;
#19622 = ORIENTED_EDGE ( 'NONE', *, *, #8817, .F. ) ;
#19623 = CARTESIAN_POINT ( 'NONE',  ( 8.905523458406561232, 12.18567386761292148, 5.103169512634847749 ) ) ;
#19624 = EDGE_CURVE ( 'NONE', #12588, #11891, #4852, .T. ) ;
#19625 = CARTESIAN_POINT ( 'NONE',  ( 49.41235866845560309, 30.56064500000000095, -26.78690084448080100 ) ) ;
#19626 = CARTESIAN_POINT ( 'NONE',  ( 9.017034975940656949, 15.28237876918361948, -3.631115729470330677 ) ) ;
#19627 = CARTESIAN_POINT ( 'NONE',  ( 20.07602185242275894, -2.531604885293976981, -15.36307167742676327 ) ) ;
#19628 = EDGE_CURVE ( 'NONE', #8439, #9259, #6062, .T. ) ;
#19629 = ORIENTED_EDGE ( 'NONE', *, *, #10715, .T. ) ;
#19630 = EDGE_CURVE ( 'NONE', #20092, #4911, #1488, .T. ) ;
#19631 = CARTESIAN_POINT ( 'NONE',  ( 6.802866078812881412, 11.05277248166000170, 4.463065346860751070 ) ) ;
#19632 = DIRECTION ( 'NONE',  ( 1.000000000000000000, 0.000000000000000000, 0.000000000000000000 ) ) ;
#19633 = ORIENTED_EDGE ( 'NONE', *, *, #14413, .F. ) ;
#19634 = EDGE_LOOP ( 'NONE', ( #14622, #21297, #13278, #11924 ) ) ;
#19635 = DIRECTION ( 'NONE',  ( 0.000000000000000000, 1.000000000000000000, 0.000000000000000000 ) ) ;
#19637 = DIRECTION ( 'NONE',  ( 0.000000000000000000, 1.000000000000000000, 0.000000000000000000 ) ) ;
#19636 = CARTESIAN_POINT ( 'NONE',  ( 1.884718254017690997, 21.29000687509540413, 4.986748289960942770 ) ) ;
#19638 = ORIENTED_EDGE ( 'NONE', *, *, #4798, .F. ) ;
#19639 = CARTESIAN_POINT ( 'NONE',  ( 4.026112509266686068, 19.40402007317530675, -0.5074809695937115839 ) ) ;
#19640 = ORIENTED_EDGE ( 'NONE', *, *, #17069, .F. ) ;
#19641 = ORIENTED_EDGE ( 'NONE', *, *, #13685, .F. ) ;
#19642 = CARTESIAN_POINT ( 'NONE',  ( 0.7492674540166441854, 12.21418807727941136, 4.792696233684067053 ) ) ;
#19643 = CIRCLE ( 'NONE', #18245, 0.5079999999999993410 ) ;
#19644 = ORIENTED_EDGE ( 'NONE', *, *, #1169, .T. ) ;
#19645 = CARTESIAN_POINT ( 'NONE',  ( 2.510246471197546292, 12.10255669127714739, 3.589570832737527528 ) ) ;
#19646 = ADVANCED_FACE ( 'NONE', ( #18441 ), #11486, .F. ) ;
#19647 = DIRECTION ( 'NONE',  ( 0.000000000000000000, 1.000000000000000000, 0.000000000000000000 ) ) ;
#19648 = LINE ( 'NONE', #21312, #2998 ) ;
#19649 = LINE ( 'NONE', #2647, #20252 ) ;
#19650 = DIRECTION ( 'NONE',  ( 0.000000000000000000, 1.000000000000000000, 0.000000000000000000 ) ) ;
#19651 = CARTESIAN_POINT ( 'NONE',  ( 3.569277441639647996, 13.57212688075029661, 8.416253947611240349 ) ) ;
#19652 = ORIENTED_EDGE ( 'NONE', *, *, #8436, .T. ) ;
#19653 = EDGE_CURVE ( 'NONE', #3095, #12537, #15143, .T. ) ;
#19654 = DIRECTION ( 'NONE',  ( -0.9685006480810792739, 0.000000000000000000, -0.2490110332224846346 ) ) ;
#19655 = DIRECTION ( 'NONE',  ( -0.3542738219355896501, 0.000000000000000000, -0.9351417320872542627 ) ) ;
#19656 = DIRECTION ( 'NONE',  ( 0.000000000000000000, 0.000000000000000000, -1.000000000000000000 ) ) ;
#19657 = DIRECTION ( 'NONE',  ( 0.000000000000000000, 1.000000000000000000, 0.000000000000000000 ) ) ;
#19658 = ORIENTED_EDGE ( 'NONE', *, *, #19630, .F. ) ;
#19659 = ORIENTED_EDGE ( 'NONE', *, *, #5454, .F. ) ;
#19660 = CARTESIAN_POINT ( 'NONE',  ( 10.01420173804988956, 20.41586353969747947, 5.057845461604397741 ) ) ;
#19661 = CIRCLE ( 'NONE', #10132, 0.7950200000000003930 ) ;
#19663 = DIRECTION ( 'NONE',  ( 0.000000000000000000, -1.000000000000000000, 0.000000000000000000 ) ) ;
#19662 = CARTESIAN_POINT ( 'NONE',  ( 17.30373842852263877, 34.52875999999999834, -12.15706637069277107 ) ) ;
#19664 = CARTESIAN_POINT ( 'NONE',  ( 12.21532007410937304, 21.58072960932728179, -1.335272812607331883 ) ) ;
#19665 = ORIENTED_EDGE ( 'NONE', *, *, #21255, .T. ) ;
#19666 = EDGE_LOOP ( 'NONE', ( #15589, #17441, #18903, #9737 ) ) ;
#19667 = CYLINDRICAL_SURFACE ( 'NONE', #17338, 0.5079999999999995630 ) ;
#19668 = CARTESIAN_POINT ( 'NONE',  ( 8.393974790171371936, 20.04483644391566699, 5.447030543808771164 ) ) ;
#19669 = CARTESIAN_POINT ( 'NONE',  ( 6.909362352619732306, 12.19147799795061182, 5.147458291921238605 ) ) ;
#19670 = EDGE_CURVE ( 'NONE', #2248, #7998, #11722, .T. ) ;
#19671 = ADVANCED_FACE ( 'NONE', ( #18545 ), #16581, .F. ) ;
#19672 = AXIS2_PLACEMENT_3D ( 'NONE', #19896, #14959, #14739 ) ;
#19673 = CARTESIAN_POINT ( 'NONE',  ( 13.62955006427684879, 22.07962435715549177, 1.866896178110612814 ) ) ;
#19674 = CARTESIAN_POINT ( 'NONE',  ( 28.97711086133420366, 0.000000000000000000, -10.71499000000000024 ) ) ;
#19675 = FACE_OUTER_BOUND ( 'NONE', #276, .T. ) ;
#19676 = CARTESIAN_POINT ( 'NONE',  ( 1.860710414810725410, 18.25211889560055667, -0.4549317619264000023 ) ) ;
#19677 = CARTESIAN_POINT ( 'NONE',  ( 0.4412527074930906457, 11.62816711700305206, 3.451613267458483403 ) ) ;
#19678 = FACE_OUTER_BOUND ( 'NONE', #17547, .T. ) ;
#19679 = CARTESIAN_POINT ( 'NONE',  ( 5.960941858113148584, 12.27647896852458231, 0.9739740074785588897 ) ) ;
#19680 = DIRECTION ( 'NONE',  ( -0.2227372614607790735, 0.000000000000000000, -0.9748785115884710528 ) ) ;
#19681 = CARTESIAN_POINT ( 'NONE',  ( 53.92979111630293687, -6.275737754352774367, -15.65141968183263899 ) ) ;
#19682 = CARTESIAN_POINT ( 'NONE',  ( 10.72409186464205355, -4.809670885807086016, -15.96177715662992824 ) ) ;
#19683 = VERTEX_POINT ( 'NONE', #13275 ) ;
#19684 = LINE ( 'NONE', #6205, #2169 ) ;
#19685 = CARTESIAN_POINT ( 'NONE',  ( 9.431633338501304920, 14.64457645186116252, 7.880854554680595925 ) ) ;
#19686 = CARTESIAN_POINT ( 'NONE',  ( 9.242220441921224605, 17.85059929941992962, -3.437012189181674060 ) ) ;
#19687 = EDGE_LOOP ( 'NONE', ( #14054, #1312, #20053, #3286 ) ) ;
#19688 = LINE ( 'NONE', #2689, #1806 ) ;
#19689 = CARTESIAN_POINT ( 'NONE',  ( 11.54223276252992747, 18.90513505042380160, -2.958155071492406751 ) ) ;
#19690 = VECTOR ( 'NONE', #1665, 1000.000000000000114 ) ;
#19691 = CARTESIAN_POINT ( 'NONE',  ( 8.131041595892833485, 21.31202829439499169, 4.830511473850858550 ) ) ;
#19692 = DIRECTION ( 'NONE',  ( -0.2868778675745010664, 0.000000000000000000, -0.9579671649362032637 ) ) ;
#19693 = CARTESIAN_POINT ( 'NONE',  ( 4.147546957899959530, 12.03379079558084186, 2.284289319685276265 ) ) ;
#19694 = CARTESIAN_POINT ( 'NONE',  ( 12.25799425556778388, 36.51313500000000545, 0.2069032437451798767 ) ) ;
#19695 = CARTESIAN_POINT ( 'NONE',  ( 54.29867169743560140, 0.000000000000000000, -30.73743011777780154 ) ) ;
#19696 = EDGE_CURVE ( 'NONE', #8373, #8830, #3191, .T. ) ;
#19697 = CARTESIAN_POINT ( 'NONE',  ( 9.610489285031960094, 13.68826078499848187, -2.403762545223697700 ) ) ;
#19698 = CARTESIAN_POINT ( 'NONE',  ( 5.080147692099665768, 18.14094701354450478, 7.664661620491963312 ) ) ;
#19699 = CARTESIAN_POINT ( 'NONE',  ( 1.567997441699468419, 12.54098868903164110, 8.004899158126836056 ) ) ;
#19700 = DIRECTION ( 'NONE',  ( 0.9685006480810792739, -0.000000000000000000, 0.2490110332224850509 ) ) ;
#19701 = AXIS2_PLACEMENT_3D ( 'NONE', #2612, #11222, #7795 ) ;
#19702 = DIRECTION ( 'NONE',  ( 0.000000000000000000, 1.000000000000000000, 0.000000000000000000 ) ) ;
#19703 = CARTESIAN_POINT ( 'NONE',  ( 6.765426361287598667, 11.37554263597316151, 2.712286843111946233 ) ) ;
#19704 = CARTESIAN_POINT ( 'NONE',  ( 53.08681243024872742, 40.07829845791615497, -16.72443647849243575 ) ) ;
#19705 = FACE_BOUND ( 'NONE', #16052, .T. ) ;
#19706 = DIRECTION ( 'NONE',  ( -0.9964481331860212121, 0.000000000000000000, 0.08420877549337300871 ) ) ;
#19707 = ORIENTED_EDGE ( 'NONE', *, *, #20541, .F. ) ;
#19708 = CARTESIAN_POINT ( 'NONE',  ( -22.75431282566211522, 40.79338547039380103, -25.41543459098148716 ) ) ;
#19709 = AXIS2_PLACEMENT_3D ( 'NONE', #1691, #20585, #8987 ) ;
#19710 = CYLINDRICAL_SURFACE ( 'NONE', #9057, 1.190625000000000711 ) ;
#19711 = ORIENTED_EDGE ( 'NONE', *, *, #6557, .T. ) ;
#19712 = CARTESIAN_POINT ( 'NONE',  ( 9.419377328995013343, 17.32343871894041953, -2.774712070466804015 ) ) ;
#19713 = CARTESIAN_POINT ( 'NONE',  ( 46.03750000000000142, 1.984375000000000000, -10.31874999999999964 ) ) ;
#19714 = LINE ( 'NONE', #13429, #15649 ) ;
#19715 = CARTESIAN_POINT ( 'NONE',  ( 11.64082572770862889, -6.986155865975274715, -15.84415276987491339 ) ) ;
#19716 = DIRECTION ( 'NONE',  ( 0.000000000000000000, -1.000000000000000000, 0.000000000000000000 ) ) ;
#19717 = ORIENTED_EDGE ( 'NONE', *, *, #8346, .T. ) ;
#19718 = CYLINDRICAL_SURFACE ( 'NONE', #10988, 1.984375000000000888 ) ;
#19719 = VECTOR ( 'NONE', #9814, 1000.000000000000000 ) ;
#19720 = ORIENTED_EDGE ( 'NONE', *, *, #17237, .F. ) ;
#19721 = DIRECTION ( 'NONE',  ( 0.000000000000000000, 1.000000000000000000, 0.000000000000000000 ) ) ;
#19722 = PRODUCT ( 'MAS-676', 'MAS-676', '', ( #1802 ) ) ;
#19723 = EDGE_CURVE ( 'NONE', #16118, #18438, #8271, .T. ) ;
#19724 = EDGE_LOOP ( 'NONE', ( #6139, #20057, #11576, #11199 ) ) ;
#19725 = CARTESIAN_POINT ( 'NONE',  ( 11.31839047608332827, 18.10733791853621710, -3.410071512985684450 ) ) ;
#19726 = CARTESIAN_POINT ( 'NONE',  ( 2.470079502529485715, 19.19535844608499175, 1.088228707528946515 ) ) ;
#19727 = VECTOR ( 'NONE', #12147, 1000.000000000000000 ) ;
#19728 = CARTESIAN_POINT ( 'NONE',  ( 46.03750000000000142, 1.984375000000000000, -10.31874999999999964 ) ) ;
#19729 = CARTESIAN_POINT ( 'NONE',  ( 8.195282804414690148, 21.33050868956278023, 5.066350132480763158 ) ) ;
#19730 =( LENGTH_UNIT ( ) NAMED_UNIT ( * ) SI_UNIT ( .MILLI., .METRE. ) );
#19731 = ORIENTED_EDGE ( 'NONE', *, *, #3697, .F. ) ;
#19732 = DIRECTION ( 'NONE',  ( 0.2490110332224848289, 0.000000000000000000, -0.9685006480810792739 ) ) ;
#19733 = DIRECTION ( 'NONE',  ( -0.9161599507719021540, -0.3242921320961419940, -0.2355537256384720723 ) ) ;
#19734 = ORIENTED_EDGE ( 'NONE', *, *, #17317, .F. ) ;
#19735 = ORIENTED_EDGE ( 'NONE', *, *, #4239, .T. ) ;
#19736 = AXIS2_PLACEMENT_3D ( 'NONE', #3936, #9110, #12457 ) ;
#19737 = CARTESIAN_POINT ( 'NONE',  ( 17.26663542346604174, 2.431245447269064108, -15.03338239065812232 ) ) ;
#19739 = DIRECTION ( 'NONE',  ( 0.000000000000000000, -1.000000000000000000, 0.000000000000000000 ) ) ;
#19738 = CARTESIAN_POINT ( 'NONE',  ( 6.194920465254885933, 21.18628736811522373, 5.570234412840648908 ) ) ;
#19740 = ORIENTED_EDGE ( 'NONE', *, *, #3410, .F. ) ;
#19741 = CARTESIAN_POINT ( 'NONE',  ( 3.516703214434496516, 14.76933982512905885, -1.184109074939236672 ) ) ;
#19742 = EDGE_CURVE ( 'NONE', #13996, #7176, #16887, .T. ) ;
#19743 = ORIENTED_EDGE ( 'NONE', *, *, #4072, .T. ) ;
#19744 = ORIENTED_EDGE ( 'NONE', *, *, #8812, .T. ) ;
#19745 = ADVANCED_FACE ( 'NONE', ( #14148 ), #13808, .F. ) ;
#19746 = VERTEX_POINT ( 'NONE', #20515 ) ;
#19747 = EDGE_CURVE ( 'NONE', #6259, #10166, #10369, .T. ) ;
#19748 = CARTESIAN_POINT ( 'NONE',  ( 2.472191904324769762, 12.13218657682475055, 3.415641386168698723 ) ) ;
#19749 = CARTESIAN_POINT ( 'NONE',  ( 4.458800082910141072, 11.90016196835719242, 3.247083169787960522 ) ) ;
#19750 = AXIS2_PLACEMENT_3D ( 'NONE', #16175, #2775, #21338 ) ;
#19751 = DIRECTION ( 'NONE',  ( -0.9129422336036123742, -0.000000000000000000, 0.4080888115384289083 ) ) ;
#19752 = CIRCLE ( 'NONE', #13773, 0.7950200000000005041 ) ;
#19753 = CARTESIAN_POINT ( 'NONE',  ( 39.11540848302676210, 37.69142280624949848, -3.773741628647232726 ) ) ;
#19754 = CARTESIAN_POINT ( 'NONE',  ( 46.03750000000000142, -14.84248999999999974, -10.31874999999999964 ) ) ;
#19755 = DIRECTION ( 'NONE',  ( 0.6050250551579474667, 0.7753173868113220069, -0.1811839737371539749 ) ) ;
#19756 = CARTESIAN_POINT ( 'NONE',  ( 3.638193303819591495, 14.51711042508261151, 8.878930407153470483 ) ) ;
#19757 = EDGE_LOOP ( 'NONE', ( #2783, #18408, #10501, #3640 ) ) ;
#19758 = PLANE ( 'NONE',  #10713 ) ;
#19759 = DIRECTION ( 'NONE',  ( -0.2490110332224850509, 0.000000000000000000, 0.9685006480810792739 ) ) ;
#19760 = CARTESIAN_POINT ( 'NONE',  ( 19.79515554403045741, 34.52875999999999834, -10.69562145279641996 ) ) ;
#19761 =( NAMED_UNIT ( * ) SI_UNIT ( $, .STERADIAN. ) SOLID_ANGLE_UNIT ( ) );
#19762 = DIRECTION ( 'NONE',  ( 0.000000000000000000, 1.000000000000000000, 0.000000000000000000 ) ) ;
#19763 = ORIENTED_EDGE ( 'NONE', *, *, #10351, .T. ) ;
#19764 = VERTEX_POINT ( 'NONE', #12782 ) ;
#19765 = CARTESIAN_POINT ( 'NONE',  ( 11.56806292758007793, 10.73085021393864125, 0.8322797596209885462 ) ) ;
#19766 = APPLICATION_CONTEXT ( 'automotive_design' ) ;
#19767 = CARTESIAN_POINT ( 'NONE',  ( 11.00610965153222054, 13.43923525470570723, -3.604247308733671495 ) ) ;
#19768 = VERTEX_POINT ( 'NONE', #12248 ) ;
#19769 = ADVANCED_FACE ( 'NONE', ( #8695 ), #15474, .T. ) ;
#19770 = EDGE_LOOP ( 'NONE', ( #10093, #9282, #13282, #4789 ) ) ;
#19771 = CARTESIAN_POINT ( 'NONE',  ( 39.00487391864218267, 37.69864044684034354, -3.894748490052650780 ) ) ;
#19772 = AXIS2_PLACEMENT_3D ( 'NONE', #16496, #1119, #3007 ) ;
#19773 = AXIS2_PLACEMENT_3D ( 'NONE', #10882, #9436, #2483 ) ;
#19774 = CARTESIAN_POINT ( 'NONE',  ( 9.093129788387537715, 17.59128346607696614, 7.060036749039768189 ) ) ;
#19775 = EDGE_CURVE ( 'NONE', #7630, #14463, #19504, .T. ) ;
#19776 = CARTESIAN_POINT ( 'NONE',  ( 3.380877013741256487, 16.38364594039518707, 8.445040901272195200 ) ) ;
#19777 = AXIS2_PLACEMENT_3D ( 'NONE', #7847, #780, #9284 ) ;
#19778 = AXIS2_PLACEMENT_3D ( 'NONE', #15809, #7604, #6163 ) ;
#19779 = EDGE_CURVE ( 'NONE', #6840, #4597, #10312, .T. ) ;
#19780 = CARTESIAN_POINT ( 'NONE',  ( 13.58266658209738331, 21.44526949881736755, 1.787837019446894216 ) ) ;
#19781 = CARTESIAN_POINT ( 'NONE',  ( 30.10940225190841701, 2.809619014187358932, -2.349505688218141319 ) ) ;
#19782 = CARTESIAN_POINT ( 'NONE',  ( 4.640211518560553472, 20.53859366438406298, 6.853938782356775228 ) ) ;
#19783 = CARTESIAN_POINT ( 'NONE',  ( 1.668587280488517788, 14.12956687025133284, 9.105894972235919482 ) ) ;
#19784 = FACE_OUTER_BOUND ( 'NONE', #21789, .T. ) ;
#19785 = ORIENTED_EDGE ( 'NONE', *, *, #4219, .T. ) ;
#19786 = CARTESIAN_POINT ( 'NONE',  ( 7.229981607529511578, 13.47123956803594069, 6.789802541014523740 ) ) ;
#19787 = CARTESIAN_POINT ( 'NONE',  ( 36.80301088673436283, 34.52875999999999834, -23.10021947667301134 ) ) ;
#19788 = DIRECTION ( 'NONE',  ( -0.5087559856598088404, 0.000000000000000000, -0.8609107660235851833 ) ) ;
#19789 = CARTESIAN_POINT ( 'NONE',  ( 13.40114476004444377, -7.897675722708163981, -15.42784453033882031 ) ) ;
#19790 = ORIENTED_EDGE ( 'NONE', *, *, #12304, .T. ) ;
#19791 = CARTESIAN_POINT ( 'NONE',  ( -12.30312499999999964, 1.984375000000000000, 8.731249999999999289 ) ) ;
#19792 = CARTESIAN_POINT ( 'NONE',  ( 12.54330750292673535, 20.52725722417916288, 5.646485819856933652 ) ) ;
#19793 = CARTESIAN_POINT ( 'NONE',  ( 9.321147220187416593, 12.33153251133805028, -2.031490842037978251 ) ) ;
#19794 = VERTEX_POINT ( 'NONE', #5723 ) ;
#19795 = EDGE_CURVE ( 'NONE', #20725, #18904, #11681, .T. ) ;
#19796 = VECTOR ( 'NONE', #5128, 1000.000000000000000 ) ;
#19797 = ADVANCED_FACE ( 'NONE', ( #13932 ), #2059, .T. ) ;
#19798 = EDGE_CURVE ( 'NONE', #14729, #10511, #15577, .T. ) ;
#19799 = CIRCLE ( 'NONE', #10269, 0.3962399999999998146 ) ;
#19800 = CARTESIAN_POINT ( 'NONE',  ( 8.733521366538639086, 20.20800283656023311, 6.430388172760417298 ) ) ;
#19801 = DIRECTION ( 'NONE',  ( -1.000000000000000000, 0.000000000000000000, 0.000000000000000000 ) ) ;
#19802 = CARTESIAN_POINT ( 'NONE',  ( 4.962249093223817020, 20.63862493749866189, 2.243063623533420259 ) ) ;
#19803 = CIRCLE ( 'NONE', #12775, 3.968750000000001776 ) ;
#19804 = SURFACE_SIDE_STYLE ('',( #21463 ) ) ;
#19805 = CARTESIAN_POINT ( 'NONE',  ( 6.787877011713288056, 19.10393197244254893, 6.711799629438941039 ) ) ;
#19806 = CARTESIAN_POINT ( 'NONE',  ( 8.505511374756364873, 34.51447250000000366, -20.97439202360551747 ) ) ;
#19807 = DIRECTION ( 'NONE',  ( 0.000000000000000000, 1.000000000000000000, 0.000000000000000000 ) ) ;
#19808 = CARTESIAN_POINT ( 'NONE',  ( 8.424495705925030720, 20.67359808219790196, 4.682861630976923095 ) ) ;
#19809 = CARTESIAN_POINT ( 'NONE',  ( 5.229436589262380863, 17.29530047414887051, 7.935297285553942537 ) ) ;
#19810 = VECTOR ( 'NONE', #9262, 1000.000000000000000 ) ;
#19811 = LINE ( 'NONE', #6445, #3171 ) ;
#19812 = CARTESIAN_POINT ( 'NONE',  ( -0.8104627873563117202, 20.56718397690614353, 3.218825348147362764 ) ) ;
#19813 = CYLINDRICAL_SURFACE ( 'NONE', #16720, 3.174999999999999378 ) ;
#19814 = CIRCLE ( 'NONE', #11008, 2.579687500000000355 ) ;
#19815 = VECTOR ( 'NONE', #7408, 1000.000000000000227 ) ;
#19816 = CARTESIAN_POINT ( 'NONE',  ( 49.09065990372640442, 1.984375000000000000, -26.70549589918839928 ) ) ;
#19817 = CARTESIAN_POINT ( 'NONE',  ( 6.768303840451392439, 11.31933340188284198, 2.707322785470000159 ) ) ;
#19818 = LINE ( 'NONE', #8320, #18898 ) ;
#19819 = CARTESIAN_POINT ( 'NONE',  ( 21.10104941149074520, -1.718252868000626155, -15.12407559264656776 ) ) ;
#19820 = FACE_OUTER_BOUND ( 'NONE', #6600, .T. ) ;
#19821 = AXIS2_PLACEMENT_3D ( 'NONE', #16048, #19759, #1091 ) ;
#19822 = ORIENTED_EDGE ( 'NONE', *, *, #18997, .F. ) ;
#19823 = LINE ( 'NONE', #6565, #805 ) ;
#19824 = DIRECTION ( 'NONE',  ( 0.000000000000000000, -1.000000000000000000, 0.000000000000000000 ) ) ;
#19825 = ORIENTED_EDGE ( 'NONE', *, *, #12085, .T. ) ;
#19826 = EDGE_CURVE ( 'NONE', #513, #10018, #21248, .T. ) ;
#19827 = CARTESIAN_POINT ( 'NONE',  ( 9.905291570324402883, 19.59492360076687589, -1.723128527427267187 ) ) ;
#19828 = CARTESIAN_POINT ( 'NONE',  ( 65.90927232300019512, 30.56064500000000095, -12.91110117861467899 ) ) ;
#19829 = CARTESIAN_POINT ( 'NONE',  ( 52.19854938732527216, 38.88803500000000213, -17.58284632693144189 ) ) ;
#19830 = CARTESIAN_POINT ( 'NONE',  ( 14.39401533775971131, 1.099227433804672138, -15.97910867269435720 ) ) ;
#19831 = CARTESIAN_POINT ( 'NONE',  ( 28.97711086133420366, 1.984375000000000000, -10.71499000000000024 ) ) ;
#19832 = VERTEX_POINT ( 'NONE', #10585 ) ;
#19833 = DIRECTION ( 'NONE',  ( 1.000000000000000000, 0.000000000000000000, 0.000000000000000000 ) ) ;
#19834 = DIRECTION ( 'NONE',  ( 0.000000000000000000, 1.000000000000000000, 0.000000000000000000 ) ) ;
#19835 = AXIS2_PLACEMENT_3D ( 'NONE', #6506, #3081, #4624 ) ;
#19836 = ORIENTED_EDGE ( 'NONE', *, *, #15180, .F. ) ;
#19837 = DIRECTION ( 'NONE',  ( -0.9129422336036127072, 0.000000000000000000, 0.4080888115384278536 ) ) ;
#19838 = VECTOR ( 'NONE', #5948, 1000.000000000000000 ) ;
#19839 = CARTESIAN_POINT ( 'NONE',  ( 14.53389803956520332, -7.867033344118881999, -17.07121685545881817 ) ) ;
#19840 = VERTEX_POINT ( 'NONE', #2706 ) ;
#19841 = CIRCLE ( 'NONE', #2908, 0.5080000000000007843 ) ;
#19842 = CARTESIAN_POINT ( 'NONE',  ( 5.783434255099849430, 12.69913397707368219, 0.2011194333812519330 ) ) ;
#19843 = CYLINDRICAL_SURFACE ( 'NONE', #5022, 0.7950199999999990608 ) ;
#19844 = CARTESIAN_POINT ( 'NONE',  ( 9.812235820622445814, 10.74839508995118109, 0.2078937617495408285 ) ) ;
#19845 = VECTOR ( 'NONE', #16680, 1000.000000000000000 ) ;
#19846 = CARTESIAN_POINT ( 'NONE',  ( 19.84048017005180142, -4.485898010009481851, -15.33043091644288225 ) ) ;
#19847 = CYLINDRICAL_SURFACE ( 'NONE', #15931, 3.968750000000000000 ) ;
#19848 = ORIENTED_EDGE ( 'NONE', *, *, #18199, .F. ) ;
#19849 = FACE_OUTER_BOUND ( 'NONE', #8466, .T. ) ;
#19850 = LINE ( 'NONE', #8025, #742 ) ;
#19851 = ORIENTED_EDGE ( 'NONE', *, *, #5878, .T. ) ;
#19852 = EDGE_LOOP ( 'NONE', ( #18559, #4961, #4735, #16271, #12060, #1439, #17543 ) ) ;
#19853 = EDGE_CURVE ( 'NONE', #17882, #20691, #21601, .T. ) ;
#19854 = VECTOR ( 'NONE', #19181, 1000.000000000000000 ) ;
#19855 = PLANE ( 'NONE',  #19032 ) ;
#19856 = AXIS2_PLACEMENT_3D ( 'NONE', #17524, #10547, #4251 ) ;
#19858 = CARTESIAN_POINT ( 'NONE',  ( -17.46249999999999858, 32.54247999999999763, 0.000000000000000000 ) ) ;
#19857 = CARTESIAN_POINT ( 'NONE',  ( -0.1826891866692206545, 17.37763432658893947, 0.05499588537583813969 ) ) ;
#19859 = VERTEX_POINT ( 'NONE', #18974 ) ;
#19860 = CARTESIAN_POINT ( 'NONE',  ( 5.347305277071898288, 21.51930324994589938, 2.982367603555873714 ) ) ;
#19861 = ORIENTED_EDGE ( 'NONE', *, *, #10826, .F. ) ;
#19862 = ORIENTED_EDGE ( 'NONE', *, *, #17647, .F. ) ;
#19863 = AXIS2_PLACEMENT_3D ( 'NONE', #7946, #16257, #16364 ) ;
#19864 = FACE_OUTER_BOUND ( 'NONE', #4707, .T. ) ;
#19865 = VERTEX_POINT ( 'NONE', #2178 ) ;
#19866 = CARTESIAN_POINT ( 'NONE',  ( 2.569241531917466848, 12.06096004062977123, 3.858983728647578104 ) ) ;
#19867 = CARTESIAN_POINT ( 'NONE',  ( 3.967314636381039428, 12.87327716067178152, 0.9669488592612511813 ) ) ;
#19868 = DIRECTION ( 'NONE',  ( 0.000000000000000000, 1.000000000000000000, 0.000000000000000000 ) ) ;
#19869 = CARTESIAN_POINT ( 'NONE',  ( 28.56548256563643662, -3.968114999999999615, -12.12873025803960658 ) ) ;
#19870 = CARTESIAN_POINT ( 'NONE',  ( 13.64200589084435578, -5.959792500000001603, -0.3187768451312169571 ) ) ;
#19871 = CARTESIAN_POINT ( 'NONE',  ( 1.676631372968138578, 14.47082764806958544, -0.3334079287914699097 ) ) ;
#19872 = ORIENTED_EDGE ( 'NONE', *, *, #19905, .T. ) ;
#19873 = FACE_OUTER_BOUND ( 'NONE', #12811, .T. ) ;
#19874 = DIRECTION ( 'NONE',  ( 0.000000000000000000, 1.000000000000000000, 0.000000000000000000 ) ) ;
#19875 = CARTESIAN_POINT ( 'NONE',  ( 1.923689137428217455, 33.48813496001219647, -20.61772871637841220 ) ) ;
#19876 = CARTESIAN_POINT ( 'NONE',  ( 53.76169727759691597, 38.28855596976028863, -15.89243902784262197 ) ) ;
#19877 = VECTOR ( 'NONE', #4067, 1000.000000000000227 ) ;
#19878 = ORIENTED_EDGE ( 'NONE', *, *, #10197, .F. ) ;
#19879 = ORIENTED_EDGE ( 'NONE', *, *, #21851, .T. ) ;
#19880 = ADVANCED_FACE ( 'NONE', ( #8920 ), #15698, .F. ) ;
#19881 = CARTESIAN_POINT ( 'NONE',  ( 7.828648054350496821, 20.67359808219790196, 4.861297291341504234 ) ) ;
#19882 = EDGE_CURVE ( 'NONE', #16262, #15380, #20175, .T. ) ;
#19884 = DIRECTION ( 'NONE',  ( 0.7421532822901579785, 0.000000000000000000, -0.6702301885068630005 ) ) ;
#19883 = CARTESIAN_POINT ( 'NONE',  ( 44.28293121686854761, 34.52875999999999834, -31.08068102505560759 ) ) ;
#19885 = ORIENTED_EDGE ( 'NONE', *, *, #1086, .F. ) ;
#19886 = ORIENTED_EDGE ( 'NONE', *, *, #20797, .F. ) ;
#19887 = CARTESIAN_POINT ( 'NONE',  ( -21.43124999999999858, 0.000000000000000000, -4.860316984116058095E-16 ) ) ;
#19888 = AXIS2_PLACEMENT_3D ( 'NONE', #15133, #3298, #16781 ) ;
#19889 = CARTESIAN_POINT ( 'NONE',  ( 9.260438503031343416, 14.54440023414849570, 6.890419401724486193 ) ) ;
#19890 = CARTESIAN_POINT ( 'NONE',  ( 3.359084728520796759, 16.63200163831436384, 8.437760029842829468 ) ) ;
#19891 = EDGE_CURVE ( 'NONE', #6728, #12014, #10702, .T. ) ;
#19892 = CARTESIAN_POINT ( 'NONE',  ( -3.042350287543033716, 28.56769750000000130, -26.17378113315171007 ) ) ;
#19893 = DIRECTION ( 'NONE',  ( 0.9685006480810792739, 0.000000000000000000, 0.2490110332224850509 ) ) ;
#19894 = CARTESIAN_POINT ( 'NONE',  ( 4.046220154711220651, 21.31561936814513913, 5.264967463508157586 ) ) ;
#19895 = CARTESIAN_POINT ( 'NONE',  ( 1.435637233034790183, 12.53020615724244102, 7.860097166555220838 ) ) ;
#19896 = CARTESIAN_POINT ( 'NONE',  ( 29.76562500000000000, 32.54502000000000095, -4.317999999999999616 ) ) ;
#19897 = ORIENTED_EDGE ( 'NONE', *, *, #10953, .T. ) ;
#19898 = CARTESIAN_POINT ( 'NONE',  ( 6.990983794162659137, 12.34350287060300211, 5.597185000230755492 ) ) ;
#19899 = CIRCLE ( 'NONE', #1552, 2.381250000000001421 ) ;
#19900 = CARTESIAN_POINT ( 'NONE',  ( 65.64431122251959039, 30.56064500000000095, -11.29787305743958115 ) ) ;
#19901 = CARTESIAN_POINT ( 'NONE',  ( 39.58386072796550081, 38.88803500000000213, -4.490541772578183100 ) ) ;
#19902 = CARTESIAN_POINT ( 'NONE',  ( 19.80365268258534783, -6.408106014325641198, -14.04632085989190493 ) ) ;
#19903 = DIRECTION ( 'NONE',  ( 0.08420877549337302259, 0.000000000000000000, 0.9964481331860212121 ) ) ;
#19904 = ORIENTED_EDGE ( 'NONE', *, *, #16755, .F. ) ;
#19905 = EDGE_CURVE ( 'NONE', #17319, #15944, #3961, .T. ) ;
#19906 = CARTESIAN_POINT ( 'NONE',  ( 9.041911633562941475, 13.32230603934784163, -2.889390931865063461 ) ) ;
#19907 = EDGE_CURVE ( 'NONE', #18598, #14787, #13160, .T. ) ;
#19908 = ADVANCED_FACE ( 'NONE', ( #18184 ), #6456, .T. ) ;
#19909 = CARTESIAN_POINT ( 'NONE',  ( 61.65536943582333151, 32.54502000000000095, -11.98363747855214712 ) ) ;
#19910 = CARTESIAN_POINT ( 'NONE',  ( 9.131607688676272261, 16.83393002257671611, -3.607777635551496775 ) ) ;
#19911 = ORIENTED_EDGE ( 'NONE', *, *, #1924, .F. ) ;
#19912 = AXIS2_PLACEMENT_3D ( 'NONE', #2144, #10549, #9914 ) ;
#19913 = CARTESIAN_POINT ( 'NONE',  ( 8.061252166635112459, 21.38919659779727311, 4.640970875387647965 ) ) ;
#19914 = CARTESIAN_POINT ( 'NONE',  ( 201.9384738932629944, 2.380615000000000148, 8.335010000000000474 ) ) ;
#19915 = CARTESIAN_POINT ( 'NONE',  ( 7.259159645424166918, 14.95027458788505648, 7.545890876313082529 ) ) ;
#19916 = CARTESIAN_POINT ( 'NONE',  ( 13.28822531734660828, 36.51313500000000545, -15.23578611614444078 ) ) ;
#19917 = DIRECTION ( 'NONE',  ( 0.000000000000000000, -1.000000000000000000, -0.000000000000000000 ) ) ;
#19918 = VECTOR ( 'NONE', #4682, 1000.000000000000227 ) ;
#19919 = CARTESIAN_POINT ( 'NONE',  ( 12.72960005895841107, 11.13394627749852361, 2.488341707347630827 ) ) ;
#19920 = ADVANCED_FACE ( 'NONE', ( #6336 ), #1257, .T. ) ;
#19921 = CIRCLE ( 'NONE', #8639, 1.587499999999999911 ) ;
#19922 = DIRECTION ( 'NONE',  ( 0.000000000000000000, 0.000000000000000000, 1.000000000000000000 ) ) ;
#19923 = CARTESIAN_POINT ( 'NONE',  ( 5.290774276891190731, 21.33523753305656001, 1.927088233765430036 ) ) ;
#19924 = EDGE_CURVE ( 'NONE', #1990, #8373, #21597, .T. ) ;
#19925 = DIRECTION ( 'NONE',  ( 0.9943660382494290406, 0.000000000000000000, -0.1060008583745199739 ) ) ;
#19926 = ADVANCED_FACE ( 'NONE', ( #16525 ), #14551, .F. ) ;
#19927 = DIRECTION ( 'NONE',  ( 0.000000000000000000, 0.000000000000000000, -1.000000000000000000 ) ) ;
#19928 = DIRECTION ( 'NONE',  ( 0.000000000000000000, -1.000000000000000000, -0.000000000000000000 ) ) ;
#19929 = CARTESIAN_POINT ( 'NONE',  ( 52.65345379380355695, 40.07865999999999929, -16.29354262597941982 ) ) ;
#19930 = CARTESIAN_POINT ( 'NONE',  ( 21.08189193827671915, -4.408480812526476278, -15.02976703352687693 ) ) ;
#19931 = DIRECTION ( 'NONE',  ( -0.000000000000000000, -1.000000000000000000, 0.000000000000000000 ) ) ;
#19932 = ORIENTED_EDGE ( 'NONE', *, *, #1220, .F. ) ;
#19933 = DIRECTION ( 'NONE',  ( -0.9959941601142527912, 0.000000000000000000, -0.08941830359777887260 ) ) ;
#19934 = CARTESIAN_POINT ( 'NONE',  ( 46.03750000000000142, 34.52875999999999834, -10.31874999999999964 ) ) ;
#19935 = VERTEX_POINT ( 'NONE', #11322 ) ;
#19936 = CARTESIAN_POINT ( 'NONE',  ( 13.10625849968711343, 16.65997537097360492, 6.401687974235077405 ) ) ;
#19937 = CARTESIAN_POINT ( 'NONE',  ( 49.41195815393805901, 0.000000000000000000, -1.411525001868561224 ) ) ;
#19938 = CARTESIAN_POINT ( 'NONE',  ( 13.64200589084435578, -6.754812500000002551, -0.3187768451312169571 ) ) ;
#19939 = CARTESIAN_POINT ( 'NONE',  ( 11.68492118186053474, -0.1802169501065840895, -16.08014746593085320 ) ) ;
#19941 = DIRECTION ( 'NONE',  ( 0.000000000000000000, 1.000000000000000000, 0.000000000000000000 ) ) ;
#19940 = CARTESIAN_POINT ( 'NONE',  ( 0.7821300450196075893, 12.31440956997844083, 6.399142672586000558 ) ) ;
#19942 = ORIENTED_EDGE ( 'NONE', *, *, #8101, .F. ) ;
#19943 = CARTESIAN_POINT ( 'NONE',  ( 29.37324403177899868, 0.000000000000000000, -10.70578951775076071 ) ) ;
#19944 = CARTESIAN_POINT ( 'NONE',  ( 3.821430202768995699, 16.87782039879526508, -0.6383179096349496096 ) ) ;
#19945 = EDGE_LOOP ( 'NONE', ( #5721, #12489 ) ) ;
#19946 = CYLINDRICAL_SURFACE ( 'NONE', #21336, 1.587499999999998579 ) ;
#19947 = CARTESIAN_POINT ( 'NONE',  ( 1.437842523326486210, 20.32886153177781807, 3.861219391056186723 ) ) ;
#19948 = CARTESIAN_POINT ( 'NONE',  ( 12.36067866020131767, -0.4634977254221773757, -17.06924854999482832 ) ) ;
#19949 = ORIENTED_EDGE ( 'NONE', *, *, #17784, .F. ) ;
#19950 = CARTESIAN_POINT ( 'NONE',  ( 6.378434091850946785, 20.04762713518370276, 0.2153161039344592409 ) ) ;
#19951 = EDGE_CURVE ( 'NONE', #14236, #20985, #19823, .T. ) ;
#19952 = DIRECTION ( 'NONE',  ( 0.000000000000000000, 1.000000000000000000, 0.000000000000000000 ) ) ;
#19953 = EDGE_CURVE ( 'NONE', #20253, #18266, #459, .T. ) ;
#19954 = CARTESIAN_POINT ( 'NONE',  ( 9.128749953449215582, 17.37245550884423295, -3.652603057860464020 ) ) ;
#19955 = CARTESIAN_POINT ( 'NONE',  ( 18.58524860537636414, -6.287937115538260180, -15.54831227122795489 ) ) ;
#19956 = B_SPLINE_CURVE_WITH_KNOTS ( 'NONE', 3,
 ( #9481, #19753, #4516, #4625, #21091, #1081, #21199, #12830, #5941, #16043, #9590, #12707 ),
 .UNSPECIFIED., .F., .F.,
 ( 4, 2, 2, 2, 2, 4 ),
 ( 0.001626748932157576297, 0.002113374744101624396, 0.002356687650073656035, 0.002600000556045687240, 0.003086626367989763961, 0.003573252179933841116 ),
 .UNSPECIFIED. ) ;
#19957 = VERTEX_POINT ( 'NONE', #16426 ) ;
#19958 = CARTESIAN_POINT ( 'NONE',  ( 10.16438117221001214, 20.46144192302394416, 4.562511949730317262 ) ) ;
#19959 = CARTESIAN_POINT ( 'NONE',  ( 7.411075239409255389, 12.62844402333576177, -1.659685333687124453 ) ) ;
#19960 = DIRECTION ( 'NONE',  ( -0.000000000000000000, -1.000000000000000000, 0.000000000000000000 ) ) ;
#19961 = ORIENTED_EDGE ( 'NONE', *, *, #18533, .F. ) ;
#19962 = ORIENTED_EDGE ( 'NONE', *, *, #14153, .F. ) ;
#19963 = CARTESIAN_POINT ( 'NONE',  ( 52.96420052373725440, 34.52875999999999834, 7.017842122255405712 ) ) ;
#19965 = CARTESIAN_POINT ( 'NONE',  ( 2.063750000000000195, 8.334374999999999645, 10.71562499999999929 ) ) ;
#19964 = CARTESIAN_POINT ( 'NONE',  ( -0.9912634196990741664, 20.56718397690614353, 3.272968853020066238 ) ) ;
#19966 = ORIENTED_EDGE ( 'NONE', *, *, #5898, .T. ) ;
#19967 = CARTESIAN_POINT ( 'NONE',  ( 7.343579971993509758, 17.90724651579188276, 8.163068317436712462 ) ) ;
#19968 = ORIENTED_EDGE ( 'NONE', *, *, #21825, .T. ) ;
#19969 = ORIENTED_EDGE ( 'NONE', *, *, #13554, .T. ) ;
#19970 = CARTESIAN_POINT ( 'NONE',  ( 32.42378190387104553, 0.000000000000000000, -18.15178106273469183 ) ) ;
#19971 = EDGE_LOOP ( 'NONE', ( #16874, #3467, #20426, #18103 ) ) ;
#19972 = CARTESIAN_POINT ( 'NONE',  ( 2.701204329178783503, 12.04454888244252686, 4.459376208058960067 ) ) ;
#19973 = EDGE_CURVE ( 'NONE', #9581, #20489, #1846, .T. ) ;
#19974 = CARTESIAN_POINT ( 'NONE',  ( 11.61875096509713678, 22.07868470824458385, 1.935183652392323594 ) ) ;
#19975 = CARTESIAN_POINT ( 'NONE',  ( -12.30312499999999964, 30.56064500000000095, 8.335010000000000474 ) ) ;
#19976 = CARTESIAN_POINT ( 'NONE',  ( 13.38171535118323341, 21.77020232253088139, 1.895702690670363122 ) ) ;
#19977 = CARTESIAN_POINT ( 'NONE',  ( 38.54095024924464497, 38.88803500000000213, -2.295677052105690841 ) ) ;
#19978 = CARTESIAN_POINT ( 'NONE',  ( 2.279600870619827191, 19.66662180573434426, 0.4729108911692707640 ) ) ;
#19979 = VERTEX_POINT ( 'NONE', #9548 ) ;
#19980 = LINE ( 'NONE', #8475, #4700 ) ;
#19981 = CARTESIAN_POINT ( 'NONE',  ( 28.56548256563643662, -1.983739999999999393, -12.12873025803960658 ) ) ;
#19982 = CYLINDRICAL_SURFACE ( 'NONE', #12807, 0.5080000000000000071 ) ;
#19983 = DIRECTION ( 'NONE',  ( -0.9964481331860212121, 0.000000000000000000, 0.08420877549337302259 ) ) ;
#19984 = EDGE_LOOP ( 'NONE', ( #9452, #9192, #19763, #11949 ) ) ;
#19985 = EDGE_LOOP ( 'NONE', ( #6425, #3385, #11686, #5077 ) ) ;
#19986 = CARTESIAN_POINT ( 'NONE',  ( 5.292458196680172477, 13.94198686298930134, -0.8460163710559848171 ) ) ;
#19987 = CARTESIAN_POINT ( 'NONE',  ( 23.41562500000000213, 32.54502000000000095, 5.159374999999999822 ) ) ;
#19988 = ORIENTED_EDGE ( 'NONE', *, *, #17775, .F. ) ;
#19989 = ORIENTED_EDGE ( 'NONE', *, *, #13636, .T. ) ;
#19990 = DIRECTION ( 'NONE',  ( -0.6702301885068628895, 0.000000000000000000, -0.7421532822901579785 ) ) ;
#19991 = ORIENTED_EDGE ( 'NONE', *, *, #8866, .T. ) ;
#19992 = CARTESIAN_POINT ( 'NONE',  ( 9.266403162818965811, 15.63651455217073760, 7.174713989175733886 ) ) ;
#19993 = EDGE_CURVE ( 'NONE', #13945, #15355, #21479, .T. ) ;
#19994 = CARTESIAN_POINT ( 'NONE',  ( 59.52193197173441774, 34.52875999999999834, -3.260183413611184911 ) ) ;
#19995 = CARTESIAN_POINT ( 'NONE',  ( 46.03750000000000142, 30.56064500000000095, -10.31874999999999964 ) ) ;
#19996 = CARTESIAN_POINT ( 'NONE',  ( 7.546616319253421246, 14.71802924512825683, 8.274008119131478267 ) ) ;
#19997 = CARTESIAN_POINT ( 'NONE',  ( 0.03891284271277922063, 12.71158167823063145, 1.613795646451485988 ) ) ;
#19998 = DIRECTION ( 'NONE',  ( -0.7421532822901579785, 0.000000000000000000, 0.6702301885068628895 ) ) ;
#19999 = AXIS2_PLACEMENT_3D ( 'NONE', #14880, #19610, #1155 ) ;
#20000 = ORIENTED_EDGE ( 'NONE', *, *, #2108, .F. ) ;
#20001 = CARTESIAN_POINT ( 'NONE',  ( 2.596685839560524123, 12.01605003366594104, 3.549272492307833371 ) ) ;
#20002 = DIRECTION ( 'NONE',  ( 0.000000000000000000, 1.000000000000000000, 0.000000000000000000 ) ) ;
#20003 = CARTESIAN_POINT ( 'NONE',  ( -13.49374999999999858, 0.000000000000000000, 0.000000000000000000 ) ) ;
#20004 = CARTESIAN_POINT ( 'NONE',  ( 13.67756757867809725, 38.48766750000000059, 2.571257636385987144 ) ) ;
#20005 = CARTESIAN_POINT ( 'NONE',  ( 42.79471501377724252, 0.000000000000000000, 5.049205022181460834 ) ) ;
#20006 = ORIENTED_EDGE ( 'NONE', *, *, #16862, .T. ) ;
#20007 = CARTESIAN_POINT ( 'NONE',  ( 11.40677969663037317, 10.98269117049956201, -1.304989702490406023 ) ) ;
#20008 = CARTESIAN_POINT ( 'NONE',  ( 9.401229242103068984, 18.82062145692554722, -3.104638505349831767 ) ) ;
#20009 = VERTEX_POINT ( 'NONE', #8100 ) ;
#20010 = CARTESIAN_POINT ( 'NONE',  ( 7.615293357427485255, 21.68393751741501063, 3.420954748769350573 ) ) ;
#20011 = CARTESIAN_POINT ( 'NONE',  ( 11.56192577415882816, 36.51313500000000545, 4.677561850332325299 ) ) ;
#20012 = CARTESIAN_POINT ( 'NONE',  ( 4.833000283041892331, 12.10687735873178283, 5.362284929865946737 ) ) ;
#20013 = EDGE_CURVE ( 'NONE', #4038, #5560, #14878, .T. ) ;
#20014 = CARTESIAN_POINT ( 'NONE',  ( 8.776506035771831193, 2.891917824018316097, -16.46252061043899673 ) ) ;
#20015 = FACE_OUTER_BOUND ( 'NONE', #6608, .T. ) ;
#20016 = EDGE_CURVE ( 'NONE', #15970, #17229, #18276, .T. ) ;
#20017 = DIRECTION ( 'NONE',  ( 0.2490110332224846346, 0.000000000000000000, -0.9685006480810792739 ) ) ;
#20018 = EDGE_CURVE ( 'NONE', #7959, #18042, #3136, .T. ) ;
#20019 = CARTESIAN_POINT ( 'NONE',  ( 9.540736633860454674, 18.39925938975357056, 7.172201154206985230 ) ) ;
#20020 = EDGE_CURVE ( 'NONE', #10927, #2943, #19609, .T. ) ;
#20021 = CARTESIAN_POINT ( 'NONE',  ( 5.853085853755254142, 13.88483174882859217, 8.144698374851461864 ) ) ;
#20022 = CARTESIAN_POINT ( 'NONE',  ( 0.7843704457339527591, 5.548947500000001476, -23.55949434567611078 ) ) ;
#20023 = DIRECTION ( 'NONE',  ( 0.000000000000000000, 1.000000000000000000, -0.000000000000000000 ) ) ;
#20024 = CARTESIAN_POINT ( 'NONE',  ( 6.760877964153869435, 11.41279743154806248, 2.716365728159965354 ) ) ;
#20025 = DIRECTION ( 'NONE',  ( 0.000000000000000000, -1.000000000000000000, 0.000000000000000000 ) ) ;
#20026 = DIRECTION ( 'NONE',  ( 0.000000000000000000, 1.000000000000000000, 0.000000000000000000 ) ) ;
#20027 = CARTESIAN_POINT ( 'NONE',  ( -17.46249999999999858, 0.000000000000000000, 0.000000000000000000 ) ) ;
#20028 = AXIS2_PLACEMENT_3D ( 'NONE', #8615, #3874, #7068 ) ;
#20029 = ORIENTED_EDGE ( 'NONE', *, *, #5473, .F. ) ;
#20030 = CARTESIAN_POINT ( 'NONE',  ( -2.607150795738780058, 0.000000000000000000, 8.731885000000000119 ) ) ;
#20031 = VERTEX_POINT ( 'NONE', #11645 ) ;
#20032 = CARTESIAN_POINT ( 'NONE',  ( 13.16751444918752689, 14.99951941989845317, 6.240119134003139223 ) ) ;
#20033 = LINE ( 'NONE', #11444, #16934 ) ;
#20034 = CARTESIAN_POINT ( 'NONE',  ( 19.43502434582083183, -5.355863433658462291, -14.20139972047578958 ) ) ;
#20035 = LINE ( 'NONE', #6238, #3175 ) ;
#20036 = ORIENTED_EDGE ( 'NONE', *, *, #8412, .T. ) ;
#20037 = DIRECTION ( 'NONE',  ( 0.000000000000000000, 0.000000000000000000, 1.000000000000000000 ) ) ;
#20038 = EDGE_CURVE ( 'NONE', #16397, #1525, #14668, .T. ) ;
#20039 = DIRECTION ( 'NONE',  ( -0.000000000000000000, -1.000000000000000000, 0.000000000000000000 ) ) ;
#20040 = ORIENTED_EDGE ( 'NONE', *, *, #3846, .F. ) ;
#20041 = CARTESIAN_POINT ( 'NONE',  ( 6.019093303612395474, 11.41279792062686127, 2.938509629527338074 ) ) ;
#20042 = EDGE_CURVE ( 'NONE', #16209, #10716, #434, .T. ) ;
#20043 = CIRCLE ( 'NONE', #18632, 3.970019999999998550 ) ;
#20044 = CARTESIAN_POINT ( 'NONE',  ( 14.45661145792178992, 1.227394729573359822, -16.40995970328339126 ) ) ;
#20045 = VERTEX_POINT ( 'NONE', #20030 ) ;
#20046 = CARTESIAN_POINT ( 'NONE',  ( 13.89594832754920084, 20.92845091260043944, 3.355964666133559593 ) ) ;
#20047 = ADVANCED_FACE ( 'NONE', ( #16210 ), #13003, .F. ) ;
#20048 = CARTESIAN_POINT ( 'NONE',  ( 3.709026512405631415, 20.56944361589559023, 4.257456878692176261 ) ) ;
#20049 = CARTESIAN_POINT ( 'NONE',  ( 12.25799425556778388, -1.983739999999999393, 0.2069032437451798767 ) ) ;
#20050 = CARTESIAN_POINT ( 'NONE',  ( 6.892679051309891669, 11.28692669747560018, 5.056475153849492976 ) ) ;
#20051 = CARTESIAN_POINT ( 'NONE',  ( -0.1652886651045968047, 14.27591886420808187, 0.4930659400215714472 ) ) ;
#20052 = CARTESIAN_POINT ( 'NONE',  ( 11.87648273465751281, -3.010377447276169072, -16.82793462644801963 ) ) ;
#20053 = ORIENTED_EDGE ( 'NONE', *, *, #210, .F. ) ;
#20054 = CARTESIAN_POINT ( 'NONE',  ( 8.514924039564494507, 20.49847539968255461, 0.1707108281186896503 ) ) ;
#20055 = CARTESIAN_POINT ( 'NONE',  ( 6.509677182189260058, 10.79806832651256165, 3.221000148203756464 ) ) ;
#20056 = CARTESIAN_POINT ( 'NONE',  ( 38.96520571134880129, -5.166360000000000952, -3.938444168234590315 ) ) ;
#20057 = ORIENTED_EDGE ( 'NONE', *, *, #12642, .T. ) ;
#20058 = EDGE_LOOP ( 'NONE', ( #2435, #16482, #17896, #10841 ) ) ;
#20059 = CIRCLE ( 'NONE', #12316, 0.3962399999999995925 ) ;
#20060 = CARTESIAN_POINT ( 'NONE',  ( 61.83151161312219557, -1.983739999999999837, -0.3645647634491749334 ) ) ;
#20062 = DIRECTION ( 'NONE',  ( -0.9579671649362033747, 0.000000000000000000, 0.2868778675745011220 ) ) ;
#20061 = CARTESIAN_POINT ( 'NONE',  ( 4.068900827735927095, 11.26224364954182100, 2.021667420744689636 ) ) ;
#20063 = EDGE_LOOP ( 'NONE', ( #4414, #13335, #18492, #56 ) ) ;
#20064 = CARTESIAN_POINT ( 'NONE',  ( 6.418448462341823202, 20.87337156576220210, 5.890648785273186583 ) ) ;
#20065 = EDGE_CURVE ( 'NONE', #20863, #20753, #2933, .T. ) ;
#20066 = VERTEX_POINT ( 'NONE', #18816 ) ;
#20067 = EDGE_CURVE ( 'NONE', #5196, #19435, #16840, .T. ) ;
#20068 = EDGE_CURVE ( 'NONE', #14783, #8133, #8533, .T. ) ;
#20069 = VERTEX_POINT ( 'NONE', #3683 ) ;
#20070 = CARTESIAN_POINT ( 'NONE',  ( 0.2977117155517410851, 12.86857687641943748, 2.662936448039754378 ) ) ;
#20071 = AXIS2_PLACEMENT_3D ( 'NONE', #12206, #20249, #15427 ) ;
#20072 = DIRECTION ( 'NONE',  ( 0.9579671649362032637, 0.000000000000000000, -0.2868778675745010664 ) ) ;
#20073 = ORIENTED_EDGE ( 'NONE', *, *, #9263, .F. ) ;
#20074 = CARTESIAN_POINT ( 'NONE',  ( 8.304011643298727208, 21.33440546750962241, 5.035657290636697425 ) ) ;
#20075 = AXIS2_PLACEMENT_3D ( 'NONE', #10252, #16999, #6937 ) ;
#20076 = DIRECTION ( 'NONE',  ( 0.1831666983862991482, 0.000000000000000000, -0.9830818687180954418 ) ) ;
#20077 = CARTESIAN_POINT ( 'NONE',  ( 29.36874999999999858, 9.921875000000000000, 8.731249999999999289 ) ) ;
#20078 = CARTESIAN_POINT ( 'NONE',  ( 1.661827395509540395, 14.91648660468646170, -0.4852861473593332309 ) ) ;
#20079 = ADVANCED_FACE ( 'NONE', ( #13877, #8420 ), #15314, .T. ) ;
#20080 = ORIENTED_EDGE ( 'NONE', *, *, #14472, .T. ) ;
#20081 = CARTESIAN_POINT ( 'NONE',  ( -1.427050033073577806, 25.39269750000000059, -23.44038945102687066 ) ) ;
#20082 = DIRECTION ( 'NONE',  ( -0.3697464814795229371, 0.9291326812858928808, 0.000000000000000000 ) ) ;
#20083 = CARTESIAN_POINT ( 'NONE',  ( 26.59062499999999929, 1.984375000000000000, 8.335010000000000474 ) ) ;
#20084 = AXIS2_PLACEMENT_3D ( 'NONE', #21690, #11627, #6548 ) ;
#20085 = CARTESIAN_POINT ( 'NONE',  ( 53.49555360346280963, 37.84815426416190576, -16.24526707472953291 ) ) ;
#20086 = ORIENTED_EDGE ( 'NONE', *, *, #7107, .F. ) ;
#20087 = ORIENTED_EDGE ( 'NONE', *, *, #20399, .F. ) ;
#20088 = CARTESIAN_POINT ( 'NONE',  ( 9.577851990202844945, 18.90452467200534414, -2.283339625814639895 ) ) ;
#20089 = FACE_OUTER_BOUND ( 'NONE', #18421, .T. ) ;
#20090 = ORIENTED_EDGE ( 'NONE', *, *, #18624, .F. ) ;
#20091 = ADVANCED_BREP_SHAPE_REPRESENTATION ( '', ( #13947, #2234 ), #652 ) ;
#20092 = VERTEX_POINT ( 'NONE', #6988 ) ;
#20093 = ADVANCED_FACE ( 'NONE', ( #18704 ), #24, .T. ) ;
#20094 = CARTESIAN_POINT ( 'NONE',  ( 29.76562500000000000, 30.56064500000000095, -4.317999999999999616 ) ) ;
#20095 = ORIENTED_EDGE ( 'NONE', *, *, #13178, .T. ) ;
#20096 = CARTESIAN_POINT ( 'NONE',  ( 9.178319404383161739, 13.53135455853282210, 6.346539953116446142 ) ) ;
#20097 = DIRECTION ( 'NONE',  ( 0.000000000000000000, -1.000000000000000000, -0.000000000000000000 ) ) ;
#20098 = CARTESIAN_POINT ( 'NONE',  ( 31.83819605565793509, 34.52875999999999834, -4.158220719828246814 ) ) ;
#20099 = LINE ( 'NONE', #15496, #170 ) ;
#20100 = CARTESIAN_POINT ( 'NONE',  ( 0.6295142619741483925, 20.10391746901840548, 1.699101084138331830 ) ) ;
#20101 = CIRCLE ( 'NONE', #13131, 30.16249999999999787 ) ;
#20102 = ORIENTED_EDGE ( 'NONE', *, *, #3559, .T. ) ;
#20103 = CARTESIAN_POINT ( 'NONE',  ( 5.715457615665387792, 20.82992769506763864, 3.705818051953985393 ) ) ;
#20104 = CARTESIAN_POINT ( 'NONE',  ( 9.256853431388732290, -1.983739999999999393, -17.09316853730597074 ) ) ;
#20105 = CARTESIAN_POINT ( 'NONE',  ( 28.38195592936287781, 2.770822500000000854, -13.81504834214261024 ) ) ;
#20106 = DIRECTION ( 'NONE',  ( 0.2490110332224850509, 0.000000000000000000, -0.9685006480810792739 ) ) ;
#20107 = CARTESIAN_POINT ( 'NONE',  ( 39.62791084302666178, 0.000000000000000000, -24.65774797299118859 ) ) ;
#20108 = ORIENTED_EDGE ( 'NONE', *, *, #1355, .T. ) ;
#20109 = CARTESIAN_POINT ( 'NONE',  ( 12.61930858051215232, 11.34183091107056107, 4.682723716983176132 ) ) ;
#20110 = CARTESIAN_POINT ( 'NONE',  ( 11.33230897168458462, 22.03951179526607973, 2.056163920724246807 ) ) ;
#20111 = ORIENTED_EDGE ( 'NONE', *, *, #16264, .F. ) ;
#20112 = STYLED_ITEM ( 'NONE', ( #16655 ), #13288 ) ;
#20113 = ADVANCED_FACE ( 'NONE', ( #17055 ), #1901, .F. ) ;
#20114 = CARTESIAN_POINT ( 'NONE',  ( 6.285968434040493769, 20.60167272699510121, -0.1906146123162393569 ) ) ;
#20115 = DIRECTION ( 'NONE',  ( 0.000000000000000000, 1.000000000000000000, -0.000000000000000000 ) ) ;
#20116 = DIRECTION ( 'NONE',  ( -0.2490110332224850509, 0.000000000000000000, 0.9685006480810792739 ) ) ;
#20117 = AXIS2_PLACEMENT_3D ( 'NONE', #3554, #10293, #21793 ) ;
#20118 = CARTESIAN_POINT ( 'NONE',  ( -16.07247711516169275, 35.13319853559599437, -10.44681224123558039 ) ) ;
#20119 = ADVANCED_FACE ( 'NONE', ( #12093 ), #15529, .T. ) ;
#20120 = CARTESIAN_POINT ( 'NONE',  ( 9.989334639727749376, 19.11784201969034314, -2.771333082350681210 ) ) ;
#20121 = AXIS2_PLACEMENT_3D ( 'NONE', #18735, #507, #15677 ) ;
#20122 = VECTOR ( 'NONE', #19706, 1000.000000000000000 ) ;
#20123 = CARTESIAN_POINT ( 'NONE',  ( 18.49922743714299855, 40.07707250000000698, -18.40490942454099965 ) ) ;
#20124 = CARTESIAN_POINT ( 'NONE',  ( 7.614894075436263954, 16.64415285869171868, 8.470436859809918673 ) ) ;
#20125 = LINE ( 'NONE', #20022, #6472 ) ;
#20126 = CARTESIAN_POINT ( 'NONE',  ( -3.845402119898529758, 3.961447500000001565, -31.39393985263922460 ) ) ;
#20127 = CYLINDRICAL_SURFACE ( 'NONE', #4415, 0.7950200000000005041 ) ;
#20128 = DIRECTION ( 'NONE',  ( 0.000000000000000000, -1.000000000000000000, 0.000000000000000000 ) ) ;
#20129 = CARTESIAN_POINT ( 'NONE',  ( 11.57088620211501784, -5.974813487921917243, -17.02130989707151443 ) ) ;
#20130 = AXIS2_PLACEMENT_3D ( 'NONE', #3373, #16852, #8430 ) ;
#20131 = VECTOR ( 'NONE', #21546, 1000.000000000000114 ) ;
#20132 = ORIENTED_EDGE ( 'NONE', *, *, #8715, .T. ) ;
#20133 = AXIS2_PLACEMENT_3D ( 'NONE', #14365, #2635, #17788 ) ;
#20134 = CARTESIAN_POINT ( 'NONE',  ( -20.57102662672950544, 34.31794000000000011, 0.6462872510839712259 ) ) ;
#20135 = DIRECTION ( 'NONE',  ( 0.05085730733808393328, 0.000000000000000000, -0.9987059298363656357 ) ) ;
#20136 = EDGE_CURVE ( 'NONE', #9564, #9371, #15095, .T. ) ;
#20137 = CARTESIAN_POINT ( 'NONE',  ( 12.63173874750594550, 11.64128040312364298, 3.463609067284325160 ) ) ;
#20138 = CARTESIAN_POINT ( 'NONE',  ( 52.96420052373725440, -1.983739999999999837, 7.017842122255405712 ) ) ;
#20139 = DIRECTION ( 'NONE',  ( 0.9685006480810794960, 0.000000000000000000, 0.2490110332224836354 ) ) ;
#20140 = ADVANCED_FACE ( 'NONE', ( #4811 ), #3042, .T. ) ;
#20141 = CARTESIAN_POINT ( 'NONE',  ( 12.36142327289271847, -0.5412543480279620178, -16.62211206573401512 ) ) ;
#20143 = DIRECTION ( 'NONE',  ( 0.000000000000000000, 0.000000000000000000, -1.000000000000000000 ) ) ;
#20142 = CARTESIAN_POINT ( 'NONE',  ( 4.285612585934864605, 11.69375961036644362, 3.894991824665326785 ) ) ;
#20144 = ORIENTED_EDGE ( 'NONE', *, *, #7042, .F. ) ;
#20145 = DIRECTION ( 'NONE',  ( 0.000000000000000000, 0.000000000000000000, 1.000000000000000000 ) ) ;
#20146 = CARTESIAN_POINT ( 'NONE',  ( -7.545238043312568088, -1.594802499999999013, -33.79351368943453338 ) ) ;
#20147 = B_SPLINE_CURVE_WITH_KNOTS ( 'NONE', 3,
 ( #4258, #2488, #830, #10887, #5904, #504, #5694, #934, #4149, #20825, #14336, #3822 ),
 .UNSPECIFIED., .F., .F.,
 ( 4, 2, 2, 2, 2, 4 ),
 ( 0.0005892739765683242207, 0.001065175039931907409, 0.001303125571613693908, 0.001541076103295480624, 0.002016977166659053404, 0.002492878230022626835 ),
 .UNSPECIFIED. ) ;
#20148 = CARTESIAN_POINT ( 'NONE',  ( 6.344067149498460623, 10.92343492048921227, 2.805454655492575444 ) ) ;
#20149 = AXIS2_PLACEMENT_3D ( 'NONE', #6479, #5030, #13242 ) ;
#20150 = AXIS2_PLACEMENT_3D ( 'NONE', #17871, #18082, #7903 ) ;
#20151 = ORIENTED_EDGE ( 'NONE', *, *, #36, .T. ) ;
#20152 = CARTESIAN_POINT ( 'NONE',  ( 12.78587835270623607, 11.94669871286416196, 4.219702435597263879 ) ) ;
#20153 = CARTESIAN_POINT ( 'NONE',  ( 9.260822009384501285, 16.57983669178404895, 7.311232780123860131 ) ) ;
#20154 = CARTESIAN_POINT ( 'NONE',  ( -1.880134707694870011, 12.30439499999999953, 7.779750394130780400 ) ) ;
#20155 = CARTESIAN_POINT ( 'NONE',  ( 11.44511088290697742, 15.66517251583919901, 7.665544166514130175 ) ) ;
#20156 = CIRCLE ( 'NONE', #18764, 25.00312500000000426 ) ;
#20157 = ADVANCED_FACE ( 'NONE', ( #4704 ), #9994, .T. ) ;
#20158 = CARTESIAN_POINT ( 'NONE',  ( 11.92901707314742410, -2.323620650010280286, -16.78204014074711381 ) ) ;
#20159 = EDGE_LOOP ( 'NONE', ( #12349, #17425, #2642, #2377 ) ) ;
#20160 = CARTESIAN_POINT ( 'NONE',  ( 9.698164836889990426, 20.96660354162156992, 3.328179347255785903 ) ) ;
#20161 = CARTESIAN_POINT ( 'NONE',  ( 5.482011443615976809, 17.41093948017483939, -2.183347155986513410 ) ) ;
#20162 = CYLINDRICAL_SURFACE ( 'NONE', #6410, 30.16250000000000142 ) ;
#20163 = VECTOR ( 'NONE', #9419, 1000.000000000000000 ) ;
#20164 = VERTEX_POINT ( 'NONE', #1686 ) ;
#20165 = ORIENTED_EDGE ( 'NONE', *, *, #5199, .T. ) ;
#20166 = CIRCLE ( 'NONE', #16327, 0.5080000000000011173 ) ;
#20167 = AXIS2_PLACEMENT_3D ( 'NONE', #561, #2214, #5413 ) ;
#20168 = DIRECTION ( 'NONE',  ( 0.4987171968201936645, 0.000000000000000000, -0.8667647648559603235 ) ) ;
#20169 = CARTESIAN_POINT ( 'NONE',  ( 11.64429300236424680, 20.36482133694056529, -2.863385722148856338 ) ) ;
#20170 = EDGE_CURVE ( 'NONE', #7176, #11404, #7508, .T. ) ;
#20172 = FACE_OUTER_BOUND ( 'NONE', #16088, .T. ) ;
#20171 = CARTESIAN_POINT ( 'NONE',  ( -0.4433120853942719153, 13.94977879502390294, 0.7288990453601157382 ) ) ;
#20173 = EDGE_LOOP ( 'NONE', ( #13551, #6576, #11238, #14316 ) ) ;
#20174 = CARTESIAN_POINT ( 'NONE',  ( 6.745190824350061121, 20.22278037098389802, 6.747779596029768179 ) ) ;
#20175 = CIRCLE ( 'NONE', #10669, 0.7950200000000005041 ) ;
#20176 = CARTESIAN_POINT ( 'NONE',  ( 30.86636926788154156, 28.96330250000000461, -42.59335521360503662 ) ) ;
#20177 = ORIENTED_EDGE ( 'NONE', *, *, #16803, .T. ) ;
#20178 = VECTOR ( 'NONE', #7200, 1000.000000000000000 ) ;
#20179 = EDGE_CURVE ( 'NONE', #17126, #3519, #16532, .T. ) ;
#20180 = DIRECTION ( 'NONE',  ( -0.9129422336036123742, -0.000000000000000000, 0.4080888115384289083 ) ) ;
#20181 = ORIENTED_EDGE ( 'NONE', *, *, #19624, .F. ) ;
#20182 = CIRCLE ( 'NONE', #2550, 1.190625000000000711 ) ;
#20183 = CIRCLE ( 'NONE', #21258, 0.7950199999999990608 ) ;
#20184 = CARTESIAN_POINT ( 'NONE',  ( 3.760608265104776748, 14.37317007178249639, -0.2024957564424711698 ) ) ;
#20185 = LINE ( 'NONE', #18539, #1156 ) ;
#20186 = DIRECTION ( 'NONE',  ( -0.9987059298363656357, 0.000000000000000000, -0.05085730733808393328 ) ) ;
#20187 = EDGE_CURVE ( 'NONE', #1735, #21211, #11415, .T. ) ;
#20188 = CARTESIAN_POINT ( 'NONE',  ( 39.58386072796507449, 40.07865999999999929, -4.490541772578644064 ) ) ;
#20189 = CARTESIAN_POINT ( 'NONE',  ( 2.723825491796734610, 20.67052922820899852, 1.612990099367228147 ) ) ;
#20190 = EDGE_CURVE ( 'NONE', #3431, #14260, #1145, .T. ) ;
#20191 = AXIS2_PLACEMENT_3D ( 'NONE', #4697, #4476, #9862 ) ;
#20192 = CIRCLE ( 'NONE', #14590, 0.5079999999999985638 ) ;
#20193 = ORIENTED_EDGE ( 'NONE', *, *, #4537, .T. ) ;
#20194 = CARTESIAN_POINT ( 'NONE',  ( 47.00675968526203263, -6.356984999999999886, -12.79836188810915232 ) ) ;
#20195 = DIRECTION ( 'NONE',  ( -0.2868778675745010664, 0.000000000000000000, -0.9579671649362032637 ) ) ;
#20196 = FACE_BOUND ( 'NONE', #12255, .T. ) ;
#20197 = DIRECTION ( 'NONE',  ( 0.9943660382494290406, 0.000000000000000000, -0.1060008583745199739 ) ) ;
#20199 = CARTESIAN_POINT ( 'NONE',  ( 17.33954469767427042, -6.884990403521952906, -14.58504387362480337 ) ) ;
#20198 = DIRECTION ( 'NONE',  ( 0.9685006480810792739, 0.000000000000000000, 0.2490110332224846346 ) ) ;
#20200 = ORIENTED_EDGE ( 'NONE', *, *, #4422, .F. ) ;
#20201 = ORIENTED_EDGE ( 'NONE', *, *, #13070, .F. ) ;
#20202 = CARTESIAN_POINT ( 'NONE',  ( 10.59520296648355497, 21.11368617580202312, 0.3248148419726618052 ) ) ;
#20203 = CARTESIAN_POINT ( 'NONE',  ( 44.27024749654656688, -6.356984999999999886, -8.722764363618033201 ) ) ;
#20204 = EDGE_LOOP ( 'NONE', ( #9055, #13827, #3638, #16960, #10819 ) ) ;
#20205 = AXIS2_PLACEMENT_3D ( 'NONE', #13869, #3899, #5318 ) ;
#20206 = ORIENTED_EDGE ( 'NONE', *, *, #8308, .F. ) ;
#20207 = DIRECTION ( 'NONE',  ( 0.000000000000000000, 0.000000000000000000, -1.000000000000000000 ) ) ;
#20208 = ORIENTED_EDGE ( 'NONE', *, *, #8273, .F. ) ;
#20209 = CARTESIAN_POINT ( 'NONE',  ( 9.177196879199145840, 16.94989067509651548, 7.186116761185386892 ) ) ;
#20210 = VECTOR ( 'NONE', #12635, 1000.000000000000000 ) ;
#20211 = CARTESIAN_POINT ( 'NONE',  ( -7.782183222554425406, 34.12394750000063937, -34.19446947475137932 ) ) ;
#20212 = CARTESIAN_POINT ( 'NONE',  ( 6.585898268469219552, 32.54502000000000095, 4.694966092919240275 ) ) ;
#20213 = FACE_OUTER_BOUND ( 'NONE', #13688, .T. ) ;
#20214 = CARTESIAN_POINT ( 'NONE',  ( -0.1870826769984814675, 15.70867390004682207, 0.08389080611283412925 ) ) ;
#20215 = EDGE_CURVE ( 'NONE', #20548, #9259, #18436, .T. ) ;
#20216 = CARTESIAN_POINT ( 'NONE',  ( 2.063750000000000195, 30.56064500000000095, -5.492750000000000021 ) ) ;
#20217 = ORIENTED_EDGE ( 'NONE', *, *, #7748, .T. ) ;
#20218 = CARTESIAN_POINT ( 'NONE',  ( 2.682654501809497827, 20.17421804741920255, 6.237504504152217244 ) ) ;
#20219 = CARTESIAN_POINT ( 'NONE',  ( 6.016625000000000334, 0.000000000000000000, 2.794000000000000039 ) ) ;
#20220 = CARTESIAN_POINT ( 'NONE',  ( 53.63564901804143403, -5.379280274696189856, -16.06402915141540433 ) ) ;
#20221 = CARTESIAN_POINT ( 'NONE',  ( -23.34164412188400561, -8.889364999999999739, -25.36579984571316615 ) ) ;
#20222 = ORIENTED_EDGE ( 'NONE', *, *, #5621, .F. ) ;
#20223 = CARTESIAN_POINT ( 'NONE',  ( 11.21177383612729628, 11.06331416201678053, -1.201043617887846082 ) ) ;
#20224 = AXIS2_PLACEMENT_3D ( 'NONE', #1621, #13264, #10030 ) ;
#20225 = CARTESIAN_POINT ( 'NONE',  ( 7.241402720468077092, 25.39269750000000059, -19.25049230170216319 ) ) ;
#20226 = CARTESIAN_POINT ( 'NONE',  ( 12.75798311189342904, 19.99333349299241291, 5.919898230773216419 ) ) ;
#20227 = ORIENTED_EDGE ( 'NONE', *, *, #16189, .F. ) ;
#20228 = CARTESIAN_POINT ( 'NONE',  ( 9.346550868333654449, 12.95375062105654607, 6.879218072990156863 ) ) ;
#20229 = CARTESIAN_POINT ( 'NONE',  ( 6.702786100604261499, 19.52118532600693968, 6.477837816616200506 ) ) ;
#20230 = CARTESIAN_POINT ( 'NONE',  ( 31.83819605565793509, 36.51313500000000545, -4.158220719828246814 ) ) ;
#20231 =( LENGTH_UNIT ( ) NAMED_UNIT ( * ) SI_UNIT ( .MILLI., .METRE. ) );
#20232 = VECTOR ( 'NONE', #16072, 1000.000000000000114 ) ;
#20233 = DIRECTION ( 'NONE',  ( 0.000000000000000000, 0.000000000000000000, -1.000000000000000000 ) ) ;
#20234 = CARTESIAN_POINT ( 'NONE',  ( 12.39456830054109737, 21.31987603492770234, 3.682287093270521616 ) ) ;
#20235 = CARTESIAN_POINT ( 'NONE',  ( 3.522851090697392440, 21.45407066062478307, 3.485718429601260659 ) ) ;
#20236 = CARTESIAN_POINT ( 'NONE',  ( 29.15193331460030279, 1.975802500000001904, -13.61707959051006966 ) ) ;
#20237 = EDGE_CURVE ( 'NONE', #4424, #2932, #19714, .T. ) ;
#20238 = CARTESIAN_POINT ( 'NONE',  ( 19.75589755847548190, 0.01053015255646662547, -14.87810992461211335 ) ) ;
#20239 = CARTESIAN_POINT ( 'NONE',  ( 2.890013838880071351, 20.19995037221810108, 2.193135344012238530 ) ) ;
#20240 = DIRECTION ( 'NONE',  ( 0.9685006480810794960, 0.000000000000000000, 0.2490110332224836354 ) ) ;
#20241 = CARTESIAN_POINT ( 'NONE',  ( 32.18388890846549799, -1.983739999999999837, 1.507793899792891468 ) ) ;
#20242 = CARTESIAN_POINT ( 'NONE',  ( 10.72896046581951701, -3.334328103274969202, -17.13545616160453733 ) ) ;
#20243 = AXIS2_PLACEMENT_3D ( 'NONE', #999, #7856, #3000 ) ;
#20244 = DIRECTION ( 'NONE',  ( 0.08420877549337302259, 0.000000000000000000, 0.9964481331860212121 ) ) ;
#20245 = ORIENTED_EDGE ( 'NONE', *, *, #882, .F. ) ;
#20246 = CARTESIAN_POINT ( 'NONE',  ( 9.049997712883802947, 21.82002798184797143, 1.568539052827725655 ) ) ;
#20247 = CYLINDRICAL_SURFACE ( 'NONE', #21584, 0.5953125000000000222 ) ;
#20248 = CARTESIAN_POINT ( 'NONE',  ( 13.02292903621057185, 13.07787182719316554, 5.285385277681105443 ) ) ;
#20249 = DIRECTION ( 'NONE',  ( 0.05085730733808393328, 0.000000000000000000, -0.9987059298363656357 ) ) ;
#20251 = CARTESIAN_POINT ( 'NONE',  ( 30.47347900023190803, 34.52875999999999834, -8.148724574017967015 ) ) ;
#20250 = CARTESIAN_POINT ( 'NONE',  ( 1.578471181848339011, 16.42212273390128985, -0.01596455333784975450 ) ) ;
#20252 = VECTOR ( 'NONE', #4517, 1000.000000000000000 ) ;
#20253 = VERTEX_POINT ( 'NONE', #16749 ) ;
#20254 =( NAMED_UNIT ( * ) PLANE_ANGLE_UNIT ( ) SI_UNIT ( $, .RADIAN. ) );
#20255 = CARTESIAN_POINT ( 'NONE',  ( 2.063749999357820109, 1.984315468747399835, 10.71562492933363941 ) ) ;
#20256 = CARTESIAN_POINT ( 'NONE',  ( 4.189560172702622154, 18.86334382086423389, 0.05853659215941360572 ) ) ;
#20257 = CARTESIAN_POINT ( 'NONE',  ( 6.101406733746572719, 11.05292897737530211, 2.887581558249757485 ) ) ;
#20258 = AXIS2_PLACEMENT_3D ( 'NONE', #4035, #16099, #824 ) ;
#20259 = EDGE_LOOP ( 'NONE', ( #19119, #6620, #3802, #13628 ) ) ;
#20260 = CARTESIAN_POINT ( 'NONE',  ( 11.28205105809946751, 12.85014763714888097, -2.380148793486948744 ) ) ;
#20261 = CARTESIAN_POINT ( 'NONE',  ( 9.281794360172153091, 15.41858152414332750, -2.876659026916958961 ) ) ;
#20262 = CARTESIAN_POINT ( 'NONE',  ( 1.441581025922393566, 11.71888320561318153, 6.433096701223809610 ) ) ;
#20263 = CARTESIAN_POINT ( 'NONE',  ( 6.852794591177100436, 21.59098349863498001, 1.404805785893212366 ) ) ;
#20264 = EDGE_CURVE ( 'NONE', #8219, #10254, #3224, .T. ) ;
#20265 = CARTESIAN_POINT ( 'NONE',  ( 12.23456664944783512, -4.754397903027896000, -16.81998147949391509 ) ) ;
#20266 = DIRECTION ( 'NONE',  ( 0.000000000000000000, -1.000000000000000000, 0.000000000000000000 ) ) ;
#20267 = ORIENTED_EDGE ( 'NONE', *, *, #1060, .F. ) ;
#20268 = CARTESIAN_POINT ( 'NONE',  ( 10.50551657660874838, 19.76665074817798740, 5.435994939576656471 ) ) ;
#20269 = CARTESIAN_POINT ( 'NONE',  ( 11.57780626085113518, 20.24847620595872044, -3.132666676146435236 ) ) ;
#20270 = AXIS2_PLACEMENT_3D ( 'NONE', #13721, #5284, #7066 ) ;
#20271 = EDGE_LOOP ( 'NONE', ( #9474, #1398, #8254, #3949 ) ) ;
#20272 = ORIENTED_EDGE ( 'NONE', *, *, #3140, .F. ) ;
#20273 = DIRECTION ( 'NONE',  ( 0.08420877549337300871, 0.000000000000000000, 0.9964481331860212121 ) ) ;
#20274 = CARTESIAN_POINT ( 'NONE',  ( 11.03093538129645879, 13.20899553483338629, -3.471696574638000410 ) ) ;
#20276 = CARTESIAN_POINT ( 'NONE',  ( 1.890011456816786062, -1.569666835661437165, -22.67530205718506053 ) ) ;
#20275 = CARTESIAN_POINT ( 'NONE',  ( 3.308062403515462879, 16.51832937791753864, 9.310454716487452487 ) ) ;
#20277 = VERTEX_POINT ( 'NONE', #612 ) ;
#20278 = CARTESIAN_POINT ( 'NONE',  ( 4.847387020393643553, 21.16549811554654070, 1.624554052234806756 ) ) ;
#20279 = CARTESIAN_POINT ( 'NONE',  ( 11.82678039945931481, -1.983739999999999393, -12.74436900065013667 ) ) ;
#20280 = ORIENTED_EDGE ( 'NONE', *, *, #11755, .F. ) ;
#20281 = EDGE_CURVE ( 'NONE', #20634, #1619, #15560, .T. ) ;
#20282 = LINE ( 'NONE', #3835, #14180 ) ;
#20283 = ORIENTED_EDGE ( 'NONE', *, *, #20237, .T. ) ;
#20284 = EDGE_CURVE ( 'NONE', #3881, #4736, #20492, .T. ) ;
#20285 = ADVANCED_FACE ( 'NONE', ( #6915 ), #20829, .F. ) ;
#20286 = EDGE_CURVE ( 'NONE', #19683, #14134, #20722, .T. ) ;
#20287 = DIRECTION ( 'NONE',  ( 0.2490110332224836354, 0.000000000000000000, -0.9685006480810794960 ) ) ;
#20288 = DIRECTION ( 'NONE',  ( 0.000000000000000000, 1.000000000000000000, 0.000000000000000000 ) ) ;
#20289 = DIRECTION ( 'NONE',  ( 0.000000000000000000, 1.000000000000000000, 0.000000000000000000 ) ) ;
#20290 = CARTESIAN_POINT ( 'NONE',  ( 1.772782524859966680, 13.34852099903613087, 0.2659304825361097357 ) ) ;
#20291 = FACE_OUTER_BOUND ( 'NONE', #621, .T. ) ;
#20292 = ORIENTED_EDGE ( 'NONE', *, *, #8979, .F. ) ;
#20293 = CARTESIAN_POINT ( 'NONE',  ( 53.08681243026497043, 37.69777154208443193, -16.72443647847455850 ) ) ;
#20294 = CARTESIAN_POINT ( 'NONE',  ( 12.79472653632228507, 36.51313500000000545, -13.31637763425449883 ) ) ;
#20295 = CARTESIAN_POINT ( 'NONE',  ( 46.03750000000000142, 42.06303499999999929, -10.31874999999999964 ) ) ;
#20296 = DIRECTION ( 'NONE',  ( -1.000000000000000000, 0.000000000000000000, 0.000000000000000000 ) ) ;
#20298 = CARTESIAN_POINT ( 'NONE',  ( 18.01622421214525360, -6.506453053838762379, -14.44805177597193691 ) ) ;
#20297 = LINE ( 'NONE', #3516, #7741 ) ;
#20299 = ORIENTED_EDGE ( 'NONE', *, *, #14538, .F. ) ;
#20300 = EDGE_LOOP ( 'NONE', ( #8276, #16670, #16324, #1881, #5678, #9220, #1293, #1726, #20584, #11509, #9216, #924, #14151, #3315, #18474, #5143, #11925, #7713, #11124, #19155, #20978, #16058, #2440, #5410, #17966, #3931, #3308, #7924, #4102, #8459, #16556, #557, #3499, #20553, #5198, #5581, #8357, #16329, #15885, #10054 ) ) ;
#20301 = CARTESIAN_POINT ( 'NONE',  ( 11.83589009288015070, 20.94460807410368020, 3.678752525316609123 ) ) ;
#20303 = CYLINDRICAL_SURFACE ( 'NONE', #18773, 0.5953125000000000222 ) ;
#20302 = CARTESIAN_POINT ( 'NONE',  ( -0.06419268334440733637, 17.37652828937785543, 0.02458381411575647629 ) ) ;
#20304 = ORIENTED_EDGE ( 'NONE', *, *, #6271, .T. ) ;
#20305 = VECTOR ( 'NONE', #6885, 1000.000000000000000 ) ;
#20306 = EDGE_LOOP ( 'NONE', ( #6536, #17402, #14831, #9774, #9927 ) ) ;
#20307 = FACE_OUTER_BOUND ( 'NONE', #6363, .T. ) ;
#20308 = ORIENTED_EDGE ( 'NONE', *, *, #19260, .T. ) ;
#20309 = EDGE_CURVE ( 'NONE', #227, #12039, #7146, .T. ) ;
#20310 = CARTESIAN_POINT ( 'NONE',  ( 9.235082566757867539, 16.29398304642754169, 7.224769592719947120 ) ) ;
#20311 = EDGE_CURVE ( 'NONE', #13568, #10812, #173, .T. ) ;
#20312 = DIRECTION ( 'NONE',  ( 0.000000000000000000, 1.000000000000000000, 0.000000000000000000 ) ) ;
#20313 = LINE ( 'NONE', #5182, #21676 ) ;
#20314 = FACE_OUTER_BOUND ( 'NONE', #19091, .T. ) ;
#20315 = CARTESIAN_POINT ( 'NONE',  ( 0.2982434584755015994, 11.88023445195970140, 2.816173442903336266 ) ) ;
#20316 = LINE ( 'NONE', #10164, #9086 ) ;
#20317 = VERTEX_POINT ( 'NONE', #1828 ) ;
#20318 = CARTESIAN_POINT ( 'NONE',  ( -0.5157468025401186207, 19.92362218466222146, 3.447839857233216065 ) ) ;
#20319 = FACE_OUTER_BOUND ( 'NONE', #5254, .T. ) ;
#20320 = CARTESIAN_POINT ( 'NONE',  ( 21.25660046192028929, 36.51313500000000545, -13.18703856829094079 ) ) ;
#20321 = CARTESIAN_POINT ( 'NONE',  ( -13.87568970999206108, 34.52875999999999834, -9.457638332870221376 ) ) ;
#20322 = VERTEX_POINT ( 'NONE', #13678 ) ;
#20323 = CARTESIAN_POINT ( 'NONE',  ( 6.603665676729555400, 11.36662928180900245, 5.110622262987013720 ) ) ;
#20324 = CARTESIAN_POINT ( 'NONE',  ( 12.34266837804400652, 21.04141915754960124, 4.830946881310729246 ) ) ;
#20325 = VERTEX_POINT ( 'NONE', #18849 ) ;
#20326 = ORIENTED_EDGE ( 'NONE', *, *, #8788, .T. ) ;
#20327 = CARTESIAN_POINT ( 'NONE',  ( 36.54633153140314761, -3.968114999999999615, -9.516661413425623550 ) ) ;
#20328 = CARTESIAN_POINT ( 'NONE',  ( 8.173974635451950022, 10.80123558147565177, 1.780665030357663881 ) ) ;
#20329 = CARTESIAN_POINT ( 'NONE',  ( 5.220610334371508010, 12.95168332381294185, 6.657391693586387937 ) ) ;
#20330 = FACE_OUTER_BOUND ( 'NONE', #16585, .T. ) ;
#20331 = EDGE_CURVE ( 'NONE', #19536, #19225, #16011, .T. ) ;
#20332 = CARTESIAN_POINT ( 'NONE',  ( 14.05820270259704152, 34.52875999999999834, -15.03781736451272444 ) ) ;
#20333 = CARTESIAN_POINT ( 'NONE',  ( 7.290686113713969796, 16.23916015988696060, 7.633697861233664561 ) ) ;
#20334 = ADVANCED_FACE ( 'NONE', ( #8899 ), #10345, .F. ) ;
#20335 = CARTESIAN_POINT ( 'NONE',  ( -46.55773479047372376, -10.87373999999999974, -7.870535429687039120 ) ) ;
#20336 = CARTESIAN_POINT ( 'NONE',  ( 16.12871017875626478, 32.54500158971978863, 9.894232675333643812 ) ) ;
#20337 = VECTOR ( 'NONE', #3575, 1000.000000000000114 ) ;
#20338 = CARTESIAN_POINT ( 'NONE',  ( 12.53826982310721760, 20.96877941592346062, -1.306849070834861459 ) ) ;
#20339 = CARTESIAN_POINT ( 'NONE',  ( 5.199408160299433312, 13.09519236484694282, 6.678571109076385959 ) ) ;
#20340 = CARTESIAN_POINT ( 'NONE',  ( -0.2371651909027980287, 15.59640844431605267, 0.003501526209365949521 ) ) ;
#20341 = DIRECTION ( 'NONE',  ( -0.5087559856597484442, 0.000000000000000000, -0.8609107660236209325 ) ) ;
#20342 = CARTESIAN_POINT ( 'NONE',  ( 19.69476243405869198, 0.1068750216841468093, -14.89306782011991181 ) ) ;
#20343 = CARTESIAN_POINT ( 'NONE',  ( 3.429500974719062789, 20.64447347884702211, 3.600101472896897192 ) ) ;
#20344 = DIRECTION ( 'NONE',  ( 0.7421532822901579785, 0.000000000000000000, -0.6702301885068630005 ) ) ;
#20345 = FACE_OUTER_BOUND ( 'NONE', #20756, .T. ) ;
#20346 = CARTESIAN_POINT ( 'NONE',  ( 11.73031006892683692, -6.200208593250644995, -16.99046436023803963 ) ) ;
#20347 = CARTESIAN_POINT ( 'NONE',  ( 13.28822531734660828, -1.983739999999999393, -15.23578611614444078 ) ) ;
#20348 = CARTESIAN_POINT ( 'NONE',  ( 9.799408270453200842, 21.70432287120915049, 3.636903252768435735 ) ) ;
#20349 = CARTESIAN_POINT ( 'NONE',  ( 42.66304184606194383, 34.52875999999999834, -19.22597499813143784 ) ) ;
#20350 = EDGE_LOOP ( 'NONE', ( #14424, #14587, #7523, #4273 ) ) ;
#20351 = CARTESIAN_POINT ( 'NONE',  ( 13.13205531879375521, 14.07666409302394683, 5.907529146869096692 ) ) ;
#20352 = AXIS2_PLACEMENT_3D ( 'NONE', #5595, #3952, #15471 ) ;
#20353 = CARTESIAN_POINT ( 'NONE',  ( 20.07032048071632957, -2.740790541356518339, -14.17576409110674795 ) ) ;
#20355 = DIRECTION ( 'NONE',  ( -0.06191955310929838502, 0.000000000000000000, 0.9980811434661737147 ) ) ;
#20354 = CARTESIAN_POINT ( 'NONE',  ( 5.120992095093605201, 15.72743057685165802, 8.262704913055413769 ) ) ;
#20356 = EDGE_LOOP ( 'NONE', ( #19261, #15449, #10014, #20864, #12700 ) ) ;
#20357 = SHAPE_DEFINITION_REPRESENTATION ( #13047, #15554 ) ;
#20358 = CARTESIAN_POINT ( 'NONE',  ( 2.063750000000000195, 8.334374999999999645, 8.731249999999999289 ) ) ;
#20359 = CARTESIAN_POINT ( 'NONE',  ( 4.799915934078755164, 20.26255486774721248, 1.564252215958407133 ) ) ;
#20360 = EDGE_CURVE ( 'NONE', #10557, #227, #12463, .T. ) ;
#20361 = DIRECTION ( 'NONE',  ( -0.2490110332224850231, 0.000000000000000000, 0.9685006480810791629 ) ) ;
#20362 = CARTESIAN_POINT ( 'NONE',  ( 6.166197546908935401, 11.63697354833761999, 2.910818794907168439 ) ) ;
#20363 = ORIENTED_EDGE ( 'NONE', *, *, #6431, .F. ) ;
#20364 = CARTESIAN_POINT ( 'NONE',  ( 7.819555740045376346, 12.04827940076156167, 0.2608701021987142044 ) ) ;
#20365 = CARTESIAN_POINT ( 'NONE',  ( 3.485963715524843742, 20.55826902126646516, 3.672317462111338138 ) ) ;
#20366 = CARTESIAN_POINT ( 'NONE',  ( 9.203386509245278901, 13.35056178516542325, 6.330368121291361838 ) ) ;
#20367 = CARTESIAN_POINT ( 'NONE',  ( -0.5919464516433436962, 20.48604666719226230, 3.193387457549251796 ) ) ;
#20368 = CARTESIAN_POINT ( 'NONE',  ( 12.60601076739248327, 20.52367786489136137, 5.624087213552067865 ) ) ;
#20369 = AXIS2_PLACEMENT_3D ( 'NONE', #11728, #1226, #6417 ) ;
#20370 = DIRECTION ( 'NONE',  ( 0.000000000000000000, 1.000000000000000000, -0.000000000000000000 ) ) ;
#20371 = CARTESIAN_POINT ( 'NONE',  ( 15.88496000606677150, -7.236326715571298251, -16.10278160673554382 ) ) ;
#20372 = DIRECTION ( 'NONE',  ( -0.07875956036501312318, 0.000000000000000000, 0.9968936410927243807 ) ) ;
#20373 = VERTEX_POINT ( 'NONE', #5363 ) ;
#20374 = CARTESIAN_POINT ( 'NONE',  ( 10.03169832878702117, 20.65254351994676085, 4.214616478178461634 ) ) ;
#20375 = CARTESIAN_POINT ( 'NONE',  ( 7.749636708646758798, 11.34385124051986260, -0.1345962991897982075 ) ) ;
#20376 = ORIENTED_EDGE ( 'NONE', *, *, #3156, .F. ) ;
#20377 = LINE ( 'NONE', #13786, #21195 ) ;
#20378 = CARTESIAN_POINT ( 'NONE',  ( 12.67276266913473748, 22.06958725633792184, -0.07262669481182190689 ) ) ;
#20380 = CARTESIAN_POINT ( 'NONE',  ( 1.998220421679061776, -1.515722362770699494, -22.64748046904500356 ) ) ;
#20379 = CARTESIAN_POINT ( 'NONE',  ( 3.208307485241757906, 15.46201706931346465, -1.280579935455534279 ) ) ;
#20381 = VERTEX_POINT ( 'NONE', #15679 ) ;
#20382 = CARTESIAN_POINT ( 'NONE',  ( 6.885262695410362177, 11.24414697040129063, 4.942298119348675911 ) ) ;
#20383 = EDGE_CURVE ( 'NONE', #16565, #18623, #10457, .T. ) ;
#20384 = CARTESIAN_POINT ( 'NONE',  ( 54.55586098912687731, 34.52876000000000545, -6.056925149195119040 ) ) ;
#20385 = CIRCLE ( 'NONE', #11226, 3.968750000000001776 ) ;
#20386 = ORIENTED_EDGE ( 'NONE', *, *, #17626, .F. ) ;
#20387 = CARTESIAN_POINT ( 'NONE',  ( 30.47347900023190803, -1.983739999999999837, -8.148724574017967015 ) ) ;
#20388 = ORIENTED_EDGE ( 'NONE', *, *, #17673, .T. ) ;
#20389 = PRODUCT_DEFINITION_FORMATION_WITH_SPECIFIED_SOURCE ( 'ANY', '', #18165, .NOT_KNOWN. ) ;
#20390 = CARTESIAN_POINT ( 'NONE',  ( 1.890944370799874541, 14.70949108297185148, 0.3943759294202709986 ) ) ;
#20391 = DIRECTION ( 'NONE',  ( 0.2490110332224850509, 0.000000000000000000, -0.9685006480810792739 ) ) ;
#20392 = LINE ( 'NONE', #12017, #2478 ) ;
#20393 = PLANE ( 'NONE',  #6190 ) ;
#20394 = CARTESIAN_POINT ( 'NONE',  ( 4.262462685244984506, 21.03436180001830280, 5.762487426441945892 ) ) ;
#20395 = CARTESIAN_POINT ( 'NONE',  ( 52.65345379380397617, 38.88803500000000213, -16.29354262597895087 ) ) ;
#20396 = ORIENTED_EDGE ( 'NONE', *, *, #20441, .T. ) ;
#20397 = LINE ( 'NONE', #6513, #18802 ) ;
#20398 = DIRECTION ( 'NONE',  ( 0.000000000000000000, 1.000000000000000000, 0.000000000000000000 ) ) ;
#20399 = EDGE_CURVE ( 'NONE', #10623, #4759, #21629, .T. ) ;
#20401 = CARTESIAN_POINT ( 'NONE',  ( 14.92182958034182860, -7.164932238483936011, -15.08823842692338246 ) ) ;
#20400 = FACE_OUTER_BOUND ( 'NONE', #16686, .T. ) ;
#20402 = ORIENTED_EDGE ( 'NONE', *, *, #19505, .F. ) ;
#20403 = ORIENTED_EDGE ( 'NONE', *, *, #12938, .F. ) ;
#20404 = CARTESIAN_POINT ( 'NONE',  ( 10.81178337345588325, 14.41047425500502754, -3.325797169458144076 ) ) ;
#20406 = CARTESIAN_POINT ( 'NONE',  ( 18.49922743714299855, -7.547927499999999235, -18.40490942454099965 ) ) ;
#20405 = CARTESIAN_POINT ( 'NONE',  ( 6.300769185105590253, 10.85645724975988102, 2.341303324005514330 ) ) ;
#20407 = ORIENTED_EDGE ( 'NONE', *, *, #6206, .F. ) ;
#20408 = ORIENTED_EDGE ( 'NONE', *, *, #5034, .T. ) ;
#20409 = DIRECTION ( 'NONE',  ( 0.000000000000000000, 1.000000000000000000, 0.000000000000000000 ) ) ;
#20410 = EDGE_CURVE ( 'NONE', #16128, #21341, #15295, .T. ) ;
#20411 = EDGE_LOOP ( 'NONE', ( #20090, #4169, #5416, #10794, #7529, #14574 ) ) ;
#20412 = EDGE_CURVE ( 'NONE', #5796, #14463, #20554, .T. ) ;
#20413 = CARTESIAN_POINT ( 'NONE',  ( 7.674060797080146656, 17.99804626195093604, -1.858667960427092147 ) ) ;
#20414 = AXIS2_PLACEMENT_3D ( 'NONE', #17557, #15804, #7378 ) ;
#20415 = VERTEX_POINT ( 'NONE', #9010 ) ;
#20416 = LINE ( 'NONE', #17020, #5784 ) ;
#20417 = CARTESIAN_POINT ( 'NONE',  ( 30.74535937054756829, -95.96551800000000298, -3.684081112461307317 ) ) ;
#20418 = CARTESIAN_POINT ( 'NONE',  ( 0.03294387470584737160, 17.99883169841178798, 0.2953920376092236677 ) ) ;
#20419 = DIRECTION ( 'NONE',  ( 0.000000000000000000, -1.000000000000000000, -0.000000000000000000 ) ) ;
#20420 = ORIENTED_EDGE ( 'NONE', *, *, #6904, .F. ) ;
#20421 = CARTESIAN_POINT ( 'NONE',  ( 7.439960277765663932, 14.95027458788505648, 7.491747371440758307 ) ) ;
#20422 = LINE ( 'NONE', #13300, #3234 ) ;
#20423 = CARTESIAN_POINT ( 'NONE',  ( 59.55063415577301811, 34.52875999999999834, -22.52230776719629191 ) ) ;
#20424 = DIRECTION ( 'NONE',  ( 0.000000000000000000, -1.000000000000000000, 0.000000000000000000 ) ) ;
#20425 = EDGE_CURVE ( 'NONE', #2020, #138, #717, .T. ) ;
#20426 = ORIENTED_EDGE ( 'NONE', *, *, #1951, .T. ) ;
#20427 = CARTESIAN_POINT ( 'NONE',  ( 7.105517633241734465, 12.68409469243044363, -1.498797362056894178 ) ) ;
#20428 = VECTOR ( 'NONE', #19287, 1000.000000000000000 ) ;
#20429 = CYLINDRICAL_SURFACE ( 'NONE', #20512, 1.984375000000000000 ) ;
#20430 = CARTESIAN_POINT ( 'NONE',  ( 13.20209200828312213, 17.93610798938899009, 6.956049917908053715 ) ) ;
#20431 = ORIENTED_EDGE ( 'NONE', *, *, #8537, .F. ) ;
#20432 = VERTEX_POINT ( 'NONE', #4047 ) ;
#20433 = CARTESIAN_POINT ( 'NONE',  ( 30.78626241496060700, -5.959792500000001603, -2.552201779827368622 ) ) ;
#20434 = CARTESIAN_POINT ( 'NONE',  ( 8.748152297807935796, 10.99744108201296200, 4.197803002740799094 ) ) ;
#20435 = CARTESIAN_POINT ( 'NONE',  ( 4.546966478565406256, 19.89702943876222108, 0.8570823776154778972 ) ) ;
#20436 = CARTESIAN_POINT ( 'NONE',  ( 39.26920185518109463, -7.547609999999999708, -4.208102635185587914 ) ) ;
#20437 = ADVANCED_FACE ( 'NONE', ( #16321 ), #14342, .T. ) ;
#20438 = CARTESIAN_POINT ( 'NONE',  ( 5.701877479152492434, 17.15261597397144300, -1.334721615692817220 ) ) ;
#20439 = CARTESIAN_POINT ( 'NONE',  ( 7.249888997917891764, 16.72360887485966074, 7.615665674260959861 ) ) ;
#20440 = CARTESIAN_POINT ( 'NONE',  ( 43.29176983217143260, 0.000000000000000000, 5.154088326438659884 ) ) ;
#20441 = EDGE_CURVE ( 'NONE', #8132, #14025, #8751, .T. ) ;
#20442 = AXIS2_PLACEMENT_3D ( 'NONE', #10205, #20355, #11982 ) ;
#20443 = CARTESIAN_POINT ( 'NONE',  ( 8.923014816335598454, 10.82907781979698214, 3.585810476635211241 ) ) ;
#20444 = CARTESIAN_POINT ( 'NONE',  ( 5.159236230403464241, 12.90301316724979230, 6.473078888706812251 ) ) ;
#20445 = DIRECTION ( 'NONE',  ( 0.000000000000000000, 1.000000000000000000, 0.000000000000000000 ) ) ;
#20446 = CARTESIAN_POINT ( 'NONE',  ( 1.728822989146519440, 14.62510310756713672, -0.5323761966249557220 ) ) ;
#20447 = DIRECTION ( 'NONE',  ( 0.000000000000000000, -1.000000000000000000, 0.000000000000000000 ) ) ;
#20448 = CARTESIAN_POINT ( 'NONE',  ( 11.82678039945931481, 36.51313500000000545, -12.74436900065013667 ) ) ;
#20449 = AXIS2_PLACEMENT_3D ( 'NONE', #5969, #2677, #7966 ) ;
#20450 = CARTESIAN_POINT ( 'NONE',  ( 29.36874999999999858, 9.921875000000000000, 10.71562499999999929 ) ) ;
#20451 = DIRECTION ( 'NONE',  ( -0.7334850928793775759, -0.6768732144311021548, 0.06198604769977036216 ) ) ;
#20452 = CARTESIAN_POINT ( 'NONE',  ( 10.81663693033208062, -4.065912185102875220, -17.13981703108838062 ) ) ;
#20453 = EDGE_CURVE ( 'NONE', #17468, #11383, #2218, .T. ) ;
#20454 = AXIS2_PLACEMENT_3D ( 'NONE', #15997, #4145, #10783 ) ;
#20455 = EDGE_CURVE ( 'NONE', #21745, #21204, #5042, .T. ) ;
#20456 = CARTESIAN_POINT ( 'NONE',  ( 61.81956123787853130, 0.000000000000000000, -1.238102447480925239 ) ) ;
#20457 = EDGE_CURVE ( 'NONE', #1126, #8118, #15385, .T. ) ;
#20458 = CARTESIAN_POINT ( 'NONE',  ( 31.05388211198297554, 34.52875999999999834, -15.23127950648024331 ) ) ;
#20459 = CARTESIAN_POINT ( 'NONE',  ( 11.42955962579599749, 15.93097772868936168, 7.566103074860009770 ) ) ;
#20460 = CARTESIAN_POINT ( 'NONE',  ( 20.23508918937977796, -1.359453322992689506, -14.75410208910826704 ) ) ;
#20461 = ORIENTED_EDGE ( 'NONE', *, *, #137, .F. ) ;
#20462 = CARTESIAN_POINT ( 'NONE',  ( 11.26921146954438413, 17.34425637698345923, -3.509015127993665661 ) ) ;
#20463 = CIRCLE ( 'NONE', #18652, 30.16250000000000497 ) ;
#20464 = CARTESIAN_POINT ( 'NONE',  ( 17.45896113601822464, -7.135217023119321489, -14.60636223679974499 ) ) ;
#20466 = CARTESIAN_POINT ( 'NONE',  ( 31.05388211198297554, 34.52875999999999834, -15.23127950648024331 ) ) ;
#20465 = CARTESIAN_POINT ( 'NONE',  ( 1.887498576900284109, 12.45711053362852283, 2.199572882868206847 ) ) ;
#20467 = ORIENTED_EDGE ( 'NONE', *, *, #2080, .T. ) ;
#20468 = PRODUCT_CONTEXT ( 'NONE', #16121, 'mechanical' ) ;
#20469 = CARTESIAN_POINT ( 'NONE',  ( -15.27935546639805331, 36.51313500000000545, -26.04713531390440906 ) ) ;
#20470 = CARTESIAN_POINT ( 'NONE',  ( 62.90077106633562209, 34.52875999999999834, 8.141649473166729933 ) ) ;
#20471 = AXIS2_PLACEMENT_3D ( 'NONE', #14201, #12198, #17604 ) ;
#20472 = CARTESIAN_POINT ( 'NONE',  ( 6.007916013726672055, 11.31933379639777115, 2.935026084599358764 ) ) ;
#20473 = AXIS2_PLACEMENT_3D ( 'NONE', #20027, #11643, #11319 ) ;
#20474 = CARTESIAN_POINT ( 'NONE',  ( 14.12745558458436435, 2.161156110892227034, -16.49458891264261950 ) ) ;
#20475 = ORIENTED_EDGE ( 'NONE', *, *, #12609, .T. ) ;
#20476 = CARTESIAN_POINT ( 'NONE',  ( 11.19173535783985152, 14.04501930844190660, 6.392579086694298418 ) ) ;
#20477 = CARTESIAN_POINT ( 'NONE',  ( 6.506685236307152564, 11.60683490608310109, 3.211009186061718257 ) ) ;
#20478 = CARTESIAN_POINT ( 'NONE',  ( 7.122533101144574275, 11.31448603738602188, 4.043997548448434287 ) ) ;
#20479 = CARTESIAN_POINT ( 'NONE',  ( 14.21445728800946284, 21.25436666907090455, 4.255708983630563047 ) ) ;
#20480 = CIRCLE ( 'NONE', #10978, 0.3962400000000008138 ) ;
#20481 = CARTESIAN_POINT ( 'NONE',  ( 31.05388211198297554, 0.000000000000000000, -15.23127950648024331 ) ) ;
#20482 = CARTESIAN_POINT ( 'NONE',  ( 18.56537198735102123, -0.02379517359284155642, -14.65636392506457319 ) ) ;
#20483 = PRODUCT_DEFINITION_CONTEXT ( 'detailed design', #17231, 'design' ) ;
#20484 = EDGE_CURVE ( 'NONE', #1768, #16128, #15660, .T. ) ;
#20485 = LINE ( 'NONE', #5355, #19068 ) ;
#20486 = ORIENTED_EDGE ( 'NONE', *, *, #21280, .T. ) ;
#20487 = CARTESIAN_POINT ( 'NONE',  ( 11.18224210415232456, 14.09124794490483268, 6.296053100427162263 ) ) ;
#20488 = CARTESIAN_POINT ( 'NONE',  ( 14.25886707861190317, 21.25379664657874201, 4.242019184281260458 ) ) ;
#20489 = VERTEX_POINT ( 'NONE', #5081 ) ;
#20490 = CARTESIAN_POINT ( 'NONE',  ( 9.560141457007446775, 12.54285006689521254, -1.123051139442911461 ) ) ;
#20491 = CARTESIAN_POINT ( 'NONE',  ( 35.15748561355322011, 0.000000000000000000, 0.3244898641346534163 ) ) ;
#20492 = LINE ( 'NONE', #3937, #19854 ) ;
#20494 = DIRECTION ( 'NONE',  ( -0.2868778675745010664, 0.000000000000000000, -0.9579671649362032637 ) ) ;
#20493 = CARTESIAN_POINT ( 'NONE',  ( 1.405129138340541095, 15.60105019847626551, 9.663121315511631337 ) ) ;
#20495 = ORIENTED_EDGE ( 'NONE', *, *, #6294, .F. ) ;
#20496 = CARTESIAN_POINT ( 'NONE',  ( 7.545992013913784824, 14.98089472672740108, 8.224318917088369929 ) ) ;
#20497 = CIRCLE ( 'NONE', #8153, 9.524999999999996803 ) ;
#20498 = DIRECTION ( 'NONE',  ( 0.7421532822901579785, 0.000000000000000000, -0.6702301885068628895 ) ) ;
#20499 = CIRCLE ( 'NONE', #4986, 16.66874999999998508 ) ;
#20500 = ORIENTED_EDGE ( 'NONE', *, *, #14517, .T. ) ;
#20501 = LINE ( 'NONE', #5154, #15691 ) ;
#20502 = ORIENTED_EDGE ( 'NONE', *, *, #9761, .F. ) ;
#20503 = AXIS2_PLACEMENT_3D ( 'NONE', #3411, #15257, #10143 ) ;
#20504 = CARTESIAN_POINT ( 'NONE',  ( 8.505511374756364873, 39.28205249999999893, -20.97439202360551747 ) ) ;
#20505 = DIRECTION ( 'NONE',  ( 0.000000000000000000, 1.000000000000000000, 0.000000000000000000 ) ) ;
#20506 = AXIS2_PLACEMENT_3D ( 'NONE', #20693, #809, #13882 ) ;
#20507 = CARTESIAN_POINT ( 'NONE',  ( 6.585898268469219552, 32.54502000000000095, 4.694966092919240275 ) ) ;
#20508 = CARTESIAN_POINT ( 'NONE',  ( 5.361345772312789748, 18.08181486485797151, 8.509980462542200641 ) ) ;
#20509 = EDGE_CURVE ( 'NONE', #4266, #17362, #21282, .T. ) ;
#20510 = CARTESIAN_POINT ( 'NONE',  ( 1.336161662408851036, 9.129395000000000593, 10.66779089274961123 ) ) ;
#20511 = AXIS2_PLACEMENT_3D ( 'NONE', #15068, #4873, #6202 ) ;
#20512 = AXIS2_PLACEMENT_3D ( 'NONE', #7205, #3883, #17370 ) ;
#20513 = ORIENTED_EDGE ( 'NONE', *, *, #6053, .T. ) ;
#20514 = CARTESIAN_POINT ( 'NONE',  ( 30.02465935949302533, 39.28268749999999443, -2.324128137548288731 ) ) ;
#20515 = CARTESIAN_POINT ( 'NONE',  ( 18.65312499999999929, 1.984375000000000000, 5.159374999999999822 ) ) ;
#20516 = DIRECTION ( 'NONE',  ( -0.2490110332224848011, 0.000000000000000000, 0.9685006480810792739 ) ) ;
#20518 = CARTESIAN_POINT ( 'NONE',  ( 17.50089948725670652, -6.812435342835657437, -14.55200422611872391 ) ) ;
#20517 = DIRECTION ( 'NONE',  ( 0.8334497143791951279, 0.000000000000000000, 0.5525953072558960066 ) ) ;
#20519 = ORIENTED_EDGE ( 'NONE', *, *, #10717, .T. ) ;
#20520 = ORIENTED_EDGE ( 'NONE', *, *, #2336, .F. ) ;
#20521 = AXIS2_PLACEMENT_3D ( 'NONE', #8619, #220, #3334 ) ;
#20522 = CARTESIAN_POINT ( 'NONE',  ( 12.56986601621718691, 21.56964499642510091, 0.5722652997315497148 ) ) ;
#20524 = CYLINDRICAL_SURFACE ( 'NONE', #782, 0.5080000000000013394 ) ;
#20523 = CARTESIAN_POINT ( 'NONE',  ( -0.8825336784069820473, 20.56338889613970267, 3.242279024569009405 ) ) ;
#20525 = EDGE_LOOP ( 'NONE', ( #5726, #15557, #14272, #2526, #13303, #15226, #16879, #21301, #6967, #17001, #13822, #6184, #18986, #49, #6498, #8562, #17289, #16746 ) ) ;
#20526 = CARTESIAN_POINT ( 'NONE',  ( 5.554765356073480653, 16.44746175198124405, 8.797311439034340097 ) ) ;
#20527 = ORIENTED_EDGE ( 'NONE', *, *, #3462, .F. ) ;
#20528 = DIRECTION ( 'NONE',  ( 0.2868778675745004558, 0.000000000000000000, 0.9579671649362035968 ) ) ;
#20529 = VERTEX_POINT ( 'NONE', #17132 ) ;
#20530 = CARTESIAN_POINT ( 'NONE',  ( 7.846877201118635625, 12.15104000883038537, 0.2813510595362812561 ) ) ;
#20531 = VECTOR ( 'NONE', #17105, 1000.000000000000000 ) ;
#20532 = CIRCLE ( 'NONE', #2553, 0.7950199999999993938 ) ;
#20533 = EDGE_LOOP ( 'NONE', ( #15483, #4673, #9821, #3636, #5780, #87 ) ) ;
#20534 = AXIS2_PLACEMENT_3D ( 'NONE', #3848, #20398, #7040 ) ;
#20535 = AXIS2_PLACEMENT_3D ( 'NONE', #11318, #6120, #9857 ) ;
#20536 = DIRECTION ( 'NONE',  ( 0.000000000000000000, 1.000000000000000000, 0.000000000000000000 ) ) ;
#20537 = DIRECTION ( 'NONE',  ( 0.000000000000000000, 1.000000000000000000, -0.000000000000000000 ) ) ;
#20538 = CARTESIAN_POINT ( 'NONE',  ( 49.16323787629939801, -42.42568807200000691, -27.09503225884920141 ) ) ;
#20539 = CARTESIAN_POINT ( 'NONE',  ( 1.088522589645603000, 20.85754858585166360, 2.898279402437147212 ) ) ;
#20540 = EDGE_CURVE ( 'NONE', #18861, #3318, #1972, .T. ) ;
#20541 = EDGE_CURVE ( 'NONE', #10543, #8326, #1353, .T. ) ;
#20542 = ORIENTED_EDGE ( 'NONE', *, *, #6825, .T. ) ;
#20543 = CARTESIAN_POINT ( 'NONE',  ( 6.603476639551990601, 11.57021355890683978, 2.365220911883943344 ) ) ;
#20544 = CARTESIAN_POINT ( 'NONE',  ( 30.74535937054756829, 36.51313500000000545, -3.684081112461307317 ) ) ;
#20545 = CARTESIAN_POINT ( 'NONE',  ( 39.11079947626275555, -1.983739999999999837, -27.65534212225540500 ) ) ;
#20546 = CARTESIAN_POINT ( 'NONE',  ( 20.95867805244277093, -1.145892873419149582, -15.34329086427974431 ) ) ;
#20547 = CIRCLE ( 'NONE', #10695, 1.984374999999998890 ) ;
#20548 = VERTEX_POINT ( 'NONE', #13106 ) ;
#20549 = CARTESIAN_POINT ( 'NONE',  ( 8.761638600038448743, 15.29706862181782512, -3.464711856886600660 ) ) ;
#20550 = CARTESIAN_POINT ( 'NONE',  ( -12.30312499999999964, 30.16440499999999858, 8.731249999999999289 ) ) ;
#20551 = CARTESIAN_POINT ( 'NONE',  ( 12.57654759969153702, 20.51656419951514110, 5.451503052877947120 ) ) ;
#20552 = EDGE_LOOP ( 'NONE', ( #5573, #8482, #8261, #20519 ) ) ;
#20553 = ORIENTED_EDGE ( 'NONE', *, *, #16504, .T. ) ;
#20554 = CIRCLE ( 'NONE', #18104, 3.174999999999998490 ) ;
#20555 = CARTESIAN_POINT ( 'NONE',  ( 15.47835459351327714, 38.48766750000000059, 5.813316144137728791 ) ) ;
#20556 = CARTESIAN_POINT ( 'NONE',  ( 9.221243833658917310, 12.25319662620856143, 6.274096147298578785 ) ) ;
#20557 = AXIS2_PLACEMENT_3D ( 'NONE', #12682, #2504, #15907 ) ;
#20558 = CARTESIAN_POINT ( 'NONE',  ( 5.273483451284230128, 17.31877066267591658, 8.017556808149928216 ) ) ;
#20559 = LINE ( 'NONE', #7533, #10158 ) ;
#20560 = CARTESIAN_POINT ( 'NONE',  ( 5.797071389579374845, 12.91321502391278742, 0.09936575144167419937 ) ) ;
#20561 = CARTESIAN_POINT ( 'NONE',  ( 38.97455088732246509, 40.07865999999999929, -3.928096151774917999 ) ) ;
#20562 = ADVANCED_FACE ( 'NONE', ( #11533 ), #8097, .F. ) ;
#20563 = VECTOR ( 'NONE', #14518, 1000.000000000000000 ) ;
#20564 = CARTESIAN_POINT ( 'NONE',  ( 18.07371581377308800, -3.968114999999999615, -11.95909761906105473 ) ) ;
#20565 = CARTESIAN_POINT ( 'NONE',  ( 5.729046844393140603, 13.63276237276972047, -1.556263347886826187 ) ) ;
#20566 = CARTESIAN_POINT ( 'NONE',  ( 13.36585934105912976, 21.37707621349031228, 1.842755075219712380 ) ) ;
#20567 = FACE_OUTER_BOUND ( 'NONE', #10453, .T. ) ;
#20568 = CARTESIAN_POINT ( 'NONE',  ( 1.710065114712777667, 15.58894874012881182, 9.662144323068869056 ) ) ;
#20569 = PLANE ( 'NONE',  #21292 ) ;
#20570 = ADVANCED_FACE ( 'NONE', ( #1151 ), #19605, .F. ) ;
#20571 = ADVANCED_FACE ( 'NONE', ( #7996 ), #7890, .T. ) ;
#20572 = CARTESIAN_POINT ( 'NONE',  ( 20.14958246138351683, -0.8772606718903691592, -14.78307071614850443 ) ) ;
#20573 = DIRECTION ( 'NONE',  ( 0.9999999999672709583, 8.090614674031770259E-06, 1.618640956562950034E-09 ) ) ;
#20574 = DIRECTION ( 'NONE',  ( 0.9636276526537417286, 0.000000000000000000, -0.2672484743474500268 ) ) ;
#20575 = PLANE ( 'NONE',  #17514 ) ;
#20576 = DIRECTION ( 'NONE',  ( 0.6496772031432432870, 0.000000000000000000, -0.7602101891687411683 ) ) ;
#20577 = CARTESIAN_POINT ( 'NONE',  ( 21.43124999999999858, 16.27314499999999953, 8.731249999999999289 ) ) ;
#20578 = CARTESIAN_POINT ( 'NONE',  ( 9.791419832355172659, 21.71027370924136335, 3.614944401813668495 ) ) ;
#20579 = VECTOR ( 'NONE', #2405, 1000.000000000000114 ) ;
#20580 = CARTESIAN_POINT ( 'NONE',  ( -5.863861779363051419, -1.594802499999999013, -34.80955303575778714 ) ) ;
#20581 = CARTESIAN_POINT ( 'NONE',  ( 12.16437857509334819, 11.19183223096340996, 1.439027855815902202 ) ) ;
#20582 = CARTESIAN_POINT ( 'NONE',  ( 8.011380105705496746, 34.12394749999999988, -19.05252355006962617 ) ) ;
#20583 = CARTESIAN_POINT ( 'NONE',  ( 0.1247290703374178134, 20.17339616899437971, 6.210515518518696432 ) ) ;
#20584 = ORIENTED_EDGE ( 'NONE', *, *, #4268, .T. ) ;
#20585 = DIRECTION ( 'NONE',  ( 0.000000000000000000, 0.000000000000000000, 1.000000000000000000 ) ) ;
#20586 = CARTESIAN_POINT ( 'NONE',  ( 53.08681243024872742, 40.07829845791615497, -16.72443647849243575 ) ) ;
#20587 = CARTESIAN_POINT ( 'NONE',  ( 5.070222232012492114, 20.55825108723754369, 2.267750972750755434 ) ) ;
#20588 = CARTESIAN_POINT ( 'NONE',  ( 52.49113927203449492, -6.356984999999999886, -16.14695822742181619 ) ) ;
#20589 = VECTOR ( 'NONE', #8789, 1000.000000000000114 ) ;
#20590 = CARTESIAN_POINT ( 'NONE',  ( 6.585898268469219552, 0.000000000000000000, 4.694966092919240275 ) ) ;
#20591 = ADVANCED_FACE ( 'NONE', ( #2703, #19705, #16626 ), #17960, .F. ) ;
#20592 = PRODUCT_DEFINITION ( 'UNKNOWN', '', #17599, #9214 ) ;
#20593 = CARTESIAN_POINT ( 'NONE',  ( 10.72591792739401306, -3.807102432456875629, -16.40592623193944632 ) ) ;
#20594 = ORIENTED_EDGE ( 'NONE', *, *, #2925, .F. ) ;
#20595 = CARTESIAN_POINT ( 'NONE',  ( 8.619290438615989203, 20.62750485818692070, 0.1704299149245824263 ) ) ;
#20596 = VECTOR ( 'NONE', #214, 1000.000000000000000 ) ;
#20597 = CARTESIAN_POINT ( 'NONE',  ( 10.31578413853228682, 20.34374524028692122, 4.916019394167047807 ) ) ;
#20598 = CARTESIAN_POINT ( 'NONE',  ( 0.3579321758081180915, 12.59227895038538136, 1.630876906149107519 ) ) ;
#20599 = DIRECTION ( 'NONE',  ( 0.000000000000000000, -1.000000000000000000, -0.000000000000000000 ) ) ;
#20600 = CARTESIAN_POINT ( 'NONE',  ( 9.335363283976800375, 36.51313500000000545, -14.20581391854862474 ) ) ;
#20601 = CARTESIAN_POINT ( 'NONE',  ( 14.36425966490409500, 0.8012915925827215347, -15.95786335565876968 ) ) ;
#20602 = LINE ( 'NONE', #2146, #3548 ) ;
#20603 = EDGE_LOOP ( 'NONE', ( #7688, #8501, #11353, #9631 ) ) ;
#20604 = APPLICATION_CONTEXT ( 'automotive_design' ) ;
#20605 = CARTESIAN_POINT ( 'NONE',  ( 9.388131599695491047, 12.85887757399174092, 6.947284762616122933 ) ) ;
#20606 = VECTOR ( 'NONE', #11610, 1000.000000000000000 ) ;
#20607 = VERTEX_POINT ( 'NONE', #4894 ) ;
#20608 = CARTESIAN_POINT ( 'NONE',  ( 9.951587701580805856, 11.56453706330047204, 0.6480317735763235776 ) ) ;
#20609 = DIRECTION ( 'NONE',  ( -0.7334850928793776870, -0.6768732144311019328, 0.06198604769976998052 ) ) ;
#20610 = CARTESIAN_POINT ( 'NONE',  ( 12.84835963116946722, 22.16018907189590337, 0.4163025617756601626 ) ) ;
#20612 = FACE_OUTER_BOUND ( 'NONE', #7117, .T. ) ;
#20611 = CARTESIAN_POINT ( 'NONE',  ( 3.870182538663821337, 11.34862606615942227, 2.113216645665817239 ) ) ;
#20613 = VERTEX_POINT ( 'NONE', #1469 ) ;
#20614 = CARTESIAN_POINT ( 'NONE',  ( -15.97216256926745714, -95.96551800000000298, -9.259783438096400587 ) ) ;
#20615 = ORIENTED_EDGE ( 'NONE', *, *, #10848, .F. ) ;
#20616 = ADVANCED_FACE ( 'NONE', ( #11209 ), #6562, .T. ) ;
#20617 = EDGE_CURVE ( 'NONE', #288, #11296, #13261, .T. ) ;
#20618 = CARTESIAN_POINT ( 'NONE',  ( 49.81956284419040060, 0.000000000000000000, 11.98436472153758103 ) ) ;
#20619 = ORIENTED_EDGE ( 'NONE', *, *, #7760, .F. ) ;
#20620 = DIRECTION ( 'NONE',  ( -0.2868778675745010664, 0.000000000000000000, -0.9579671649362032637 ) ) ;
#20621 = AXIS2_PLACEMENT_3D ( 'NONE', #1136, #14655, #21466 ) ;
#20622 = DIRECTION ( 'NONE',  ( 0.000000000000000000, 1.000000000000000000, 0.000000000000000000 ) ) ;
#20623 = CARTESIAN_POINT ( 'NONE',  ( 47.80475250345343596, -6.356985000000002550, -11.91473563638196786 ) ) ;
#20624 = VECTOR ( 'NONE', #20764, 1000.000000000000000 ) ;
#20625 = CARTESIAN_POINT ( 'NONE',  ( 29.19635173153840313, 1.984375000000000000, -6.218966092919240296 ) ) ;
#20626 = DIRECTION ( 'NONE',  ( 0.000000000000000000, 1.000000000000000000, 0.000000000000000000 ) ) ;
#20627 = VERTEX_POINT ( 'NONE', #13082 ) ;
#20628 = DIRECTION ( 'NONE',  ( 0.2490110332224846346, 0.000000000000000000, -0.9685006480810792739 ) ) ;
#20629 = DIRECTION ( 'NONE',  ( -0.2868778675745011220, 0.000000000000000000, -0.9579671649362034858 ) ) ;
#20630 = DIRECTION ( 'NONE',  ( -1.000000000000000000, 0.000000000000000000, 0.000000000000000000 ) ) ;
#20632 = CARTESIAN_POINT ( 'NONE',  ( 18.57850393197893624, -6.030482575976392035, -14.33843453756632158 ) ) ;
#20631 = CARTESIAN_POINT ( 'NONE',  ( 3.805353748838121053, -1.983739999999999393, -22.18284873352824960 ) ) ;
#20633 = EDGE_LOOP ( 'NONE', ( #285, #8157, #1986, #11324 ) ) ;
#20634 = VERTEX_POINT ( 'NONE', #4551 ) ;
#20635 = CARTESIAN_POINT ( 'NONE',  ( 11.25603071367706143, 18.10558555414991844, -3.386525855160758436 ) ) ;
#20637 = CARTESIAN_POINT ( 'NONE',  ( -23.01875000000000071, 1.984375000000000000, -10.31874999999999964 ) ) ;
#20636 = CARTESIAN_POINT ( 'NONE',  ( 5.651302110662487443, 15.64116283607404689, 8.852329451391270254 ) ) ;
#20638 = EDGE_LOOP ( 'NONE', ( #15375, #19090, #11797, #12239 ) ) ;
#20640 = CARTESIAN_POINT ( 'NONE',  ( 10.44501673953377896, -3.826156291150850652, -15.85328698979687445 ) ) ;
#20639 = CARTESIAN_POINT ( 'NONE',  ( 4.987524875783154954, 11.43561499633722178, 5.539610460427389249 ) ) ;
#20641 = ORIENTED_EDGE ( 'NONE', *, *, #11698, .F. ) ;
#20642 = VERTEX_POINT ( 'NONE', #3009 ) ;
#20643 = CARTESIAN_POINT ( 'NONE',  ( 8.046159076093074347, 19.48966040285201018, -1.019939477906512737 ) ) ;
#20644 = VECTOR ( 'NONE', #1624, 1000.000000000000000 ) ;
#20645 = CARTESIAN_POINT ( 'NONE',  ( 1.455225922851533182, 14.34770218287011723, 8.351802277904694094 ) ) ;
#20646 = EDGE_CURVE ( 'NONE', #16037, #14232, #8534, .T. ) ;
#20647 = EDGE_LOOP ( 'NONE', ( #19307, #14678 ) ) ;
#20648 = CARTESIAN_POINT ( 'NONE',  ( 3.430012568879817980, 15.13584884034968780, 8.277410437623871076 ) ) ;
#20649 = CARTESIAN_POINT ( 'NONE',  ( 4.479823106602060179, 0.04783660261014419796, 9.171550912739061090 ) ) ;
#20650 = FACE_OUTER_BOUND ( 'NONE', #12157, .T. ) ;
#20651 = DIRECTION ( 'NONE',  ( 0.000000000000000000, -1.000000000000000000, 0.000000000000000000 ) ) ;
#20652 = CARTESIAN_POINT ( 'NONE',  ( 1.250047875415068344, 21.00885809591095210, 3.329580551905352070 ) ) ;
#20653 = DIRECTION ( 'NONE',  ( -0.9685006480810792739, 0.000000000000000000, -0.2490110332224846346 ) ) ;
#20654 = ORIENTED_EDGE ( 'NONE', *, *, #797, .F. ) ;
#20655 = CARTESIAN_POINT ( 'NONE',  ( 0.4435595513821114499, 17.28679025579738138, 0.2841677601690540955 ) ) ;
#20656 = CARTESIAN_POINT ( 'NONE',  ( 35.47639361272155867, 1.975802500000001904, -41.40807265590733977 ) ) ;
#20657 = DIRECTION ( 'NONE',  ( 0.000000000000000000, 1.000000000000000000, 0.000000000000000000 ) ) ;
#20658 = CARTESIAN_POINT ( 'NONE',  ( -16.07247711516169275, 35.13319853559599437, -10.44681224123558039 ) ) ;
#20659 = AXIS2_PLACEMENT_3D ( 'NONE', #475, #7229, #18813 ) ;
#20660 = DIRECTION ( 'NONE',  ( 0.000000000000000000, 1.000000000000000000, 0.000000000000000000 ) ) ;
#20661 = VERTEX_POINT ( 'NONE', #21679 ) ;
#20662 = EDGE_LOOP ( 'NONE', ( #7818, #16973, #20272, #4080, #15825, #8164 ) ) ;
#20663 = CARTESIAN_POINT ( 'NONE',  ( 13.71574892877014307, 21.56570388316688280, 3.741136478433525259 ) ) ;
#20664 = DIRECTION ( 'NONE',  ( 0.000000000000000000, 1.000000000000000000, 0.000000000000000000 ) ) ;
#20665 = CARTESIAN_POINT ( 'NONE',  ( 13.06958847994923012, 11.92395113995147327, 5.272319428283388731 ) ) ;
#20666 = ORIENTED_EDGE ( 'NONE', *, *, #18457, .F. ) ;
#20667 = ORIENTED_EDGE ( 'NONE', *, *, #21692, .F. ) ;
#20668 = FACE_OUTER_BOUND ( 'NONE', #14642, .T. ) ;
#20669 = CARTESIAN_POINT ( 'NONE',  ( 8.802176959052905758, 11.07856084916381079, 4.427857316288414502 ) ) ;
#20670 = CARTESIAN_POINT ( 'NONE',  ( 1.504320668523305260, 14.30666394527731633, 8.418582497567321354 ) ) ;
#20671 = CARTESIAN_POINT ( 'NONE',  ( 24.43309469626978725, 9.340595522457139310, -0.6496488801123181389 ) ) ;
#20672 = CARTESIAN_POINT ( 'NONE',  ( 5.995197512313855448, 18.75043017290921199, -0.7670460466430296664 ) ) ;
#20673 = EDGE_CURVE ( 'NONE', #1981, #21656, #8297, .T. ) ;
#20674 = CARTESIAN_POINT ( 'NONE',  ( 1.716565355178531371, 20.41010863060546754, 4.584836742679530452 ) ) ;
#20675 = CARTESIAN_POINT ( 'NONE',  ( -5.536601939709260733, 3.961447500000001565, -30.39452380949970944 ) ) ;
#20676 = CYLINDRICAL_SURFACE ( 'NONE', #9150, 0.7950200000000000600 ) ;
#20677 = CARTESIAN_POINT ( 'NONE',  ( 13.28865384689049911, 11.60770318476056140, 4.300680844371669309 ) ) ;
#20678 = CARTESIAN_POINT ( 'NONE',  ( 4.824783279085094634, 12.04281452664502616, 4.895154947829936098 ) ) ;
#20679 = DIRECTION ( 'NONE',  ( 0.7421532822901579785, 0.000000000000000000, -0.6702301885068628895 ) ) ;
#20680 = CARTESIAN_POINT ( 'NONE',  ( 7.555694491798023549, 14.71783044265311702, 8.271986479273186532 ) ) ;
#20681 = CARTESIAN_POINT ( 'NONE',  ( 1.526914824943621962, 17.60663541863096526, 9.449669020237495332 ) ) ;
#20682 = EDGE_CURVE ( 'NONE', #19764, #1295, #11842, .T. ) ;
#20683 = FACE_OUTER_BOUND ( 'NONE', #3490, .T. ) ;
#20684 = CARTESIAN_POINT ( 'NONE',  ( 0.6811041950880551976, 19.54923001721996201, 7.409756494194279064 ) ) ;
#20685 = DIRECTION ( 'NONE',  ( 0.000000000000000000, 0.000000000000000000, 1.000000000000000000 ) ) ;
#20686 = FACE_OUTER_BOUND ( 'NONE', #1503, .T. ) ;
#20687 = CARTESIAN_POINT ( 'NONE',  ( 20.16553087357842244, -0.1900022357140263018, -14.19585043658483237 ) ) ;
#20688 = DIRECTION ( 'NONE',  ( 0.000000000000000000, 1.000000000000000000, 0.000000000000000000 ) ) ;
#20689 = LINE ( 'NONE', #10763, #6754 ) ;
#20690 = CARTESIAN_POINT ( 'NONE',  ( 8.942822476781397967, 21.77045158648074263, 1.273023891447270017 ) ) ;
#20691 = VERTEX_POINT ( 'NONE', #20321 ) ;
#20692 = EDGE_CURVE ( 'NONE', #3856, #14138, #10670, .T. ) ;
#20693 = CARTESIAN_POINT ( 'NONE',  ( 61.56621290189396944, 29.95901653600000003, -0.7977859469341201937 ) ) ;
#20694 = CARTESIAN_POINT ( 'NONE',  ( 12.21848165272913711, 11.19810920596540171, 1.671241500708527283 ) ) ;
#20695 = CARTESIAN_POINT ( 'NONE',  ( 42.35466991749225940, -9.531985000000000596, -17.94967221382040279 ) ) ;
#20696 = CARTESIAN_POINT ( 'NONE',  ( 0.6733089074914639927, 12.13066582883064193, 4.886095876978508556 ) ) ;
#20697 = EDGE_LOOP ( 'NONE', ( #6918, #19508, #13148, #13373 ) ) ;
#20698 = CONTEXT_DEPENDENT_SHAPE_REPRESENTATION ( #5504, #15362 ) ;
#20699 = EDGE_CURVE ( 'NONE', #1966, #1190, #19841, .T. ) ;
#20700 = AXIS2_PLACEMENT_3D ( 'NONE', #886, #7407, #14181 ) ;
#20701 = EDGE_CURVE ( 'NONE', #16977, #6777, #5191, .T. ) ;
#20702 = EDGE_CURVE ( 'NONE', #3268, #11564, #15631, .T. ) ;
#20703 = LINE ( 'NONE', #20590, #10049 ) ;
#20704 = CARTESIAN_POINT ( 'NONE',  ( 13.99792333881812212, 2.297051954170742150, -16.18942158505737794 ) ) ;
#20705 = ORIENTED_EDGE ( 'NONE', *, *, #3559, .F. ) ;
#20706 = CARTESIAN_POINT ( 'NONE',  ( 11.40022844353273257, 21.35256525590422072, 1.960600886665106568 ) ) ;
#20707 = CARTESIAN_POINT ( 'NONE',  ( 4.540541346939511946, 19.75650230952821929, 6.404782441630064937 ) ) ;
#20708 = CARTESIAN_POINT ( 'NONE',  ( 11.32641745410349188, 12.84969026437554085, -2.393983499798812531 ) ) ;
#20709 = CARTESIAN_POINT ( 'NONE',  ( 5.477926520976066804, 18.98716039713233883, 7.626504097506649593 ) ) ;
#20710 = CARTESIAN_POINT ( 'NONE',  ( 14.20546330549358416, 21.25379664657874201, 4.258011758049313755 ) ) ;
#20711 = CARTESIAN_POINT ( 'NONE',  ( 30.50878709810603340, 32.54502000000000095, -19.83971405306587954 ) ) ;
#20712 = LINE ( 'NONE', #5138, #5281 ) ;
#20713 = CIRCLE ( 'NONE', #11561, 0.7950200000000003930 ) ;
#20714 = EDGE_LOOP ( 'NONE', ( #651, #9139, #2528, #1556 ) ) ;
#20715 = CARTESIAN_POINT ( 'NONE',  ( 11.22190391525087350, 15.19668154793438930, 6.694160798341728835 ) ) ;
#20716 = CARTESIAN_POINT ( 'NONE',  ( 9.151190155320593433, 13.32446407270766287, -2.918248225538348173 ) ) ;
#20717 = EDGE_CURVE ( 'NONE', #15983, #20613, #8395, .T. ) ;
#20718 = CARTESIAN_POINT ( 'NONE',  ( 41.78116128337411794, -4.569743463999999200, 7.392073290253172502 ) ) ;
#20719 = ORIENTED_EDGE ( 'NONE', *, *, #16678, .T. ) ;
#20720 = CARTESIAN_POINT ( 'NONE',  ( 9.938994540168200942, 11.58108249686686264, 0.5927703295592824384 ) ) ;
#20721 = CARTESIAN_POINT ( 'NONE',  ( 53.25483508941461963, 32.54501999999999384, -5.879799058943532941 ) ) ;
#20722 = LINE ( 'NONE', #8569, #3623 ) ;
#20724 = DIRECTION ( 'NONE',  ( 0.000000000000000000, 1.000000000000000000, 0.000000000000000000 ) ) ;
#20723 = CARTESIAN_POINT ( 'NONE',  ( -0.007942533697514499169, 12.00400186595892293, 3.420830230896959812 ) ) ;
#20725 = VERTEX_POINT ( 'NONE', #8621 ) ;
#20726 = CARTESIAN_POINT ( 'NONE',  ( 6.989266892685158439, 11.43297635884717245, 5.392041351863374743 ) ) ;
#20727 = DIRECTION ( 'NONE',  ( -0.2868778675745010664, 0.000000000000000000, -0.9579671649362032637 ) ) ;
#20728 = ORIENTED_EDGE ( 'NONE', *, *, #6413, .F. ) ;
#20729 = ADVANCED_FACE ( 'NONE', ( #15397 ), #222, .F. ) ;
#20730 = CARTESIAN_POINT ( 'NONE',  ( 12.25799425556778388, -3.968114999999999615, 0.2069032437451798767 ) ) ;
#20731 = AXIS2_PLACEMENT_3D ( 'NONE', #12968, #21446, #13393 ) ;
#20732 = CARTESIAN_POINT ( 'NONE',  ( 14.60682252872488540, -7.260664136960075510, -16.51448333835476490 ) ) ;
#20733 = ORIENTED_EDGE ( 'NONE', *, *, #4842, .T. ) ;
#20734 = CARTESIAN_POINT ( 'NONE',  ( -46.55710204590916135, 38.25938500000000175, -7.870588902259476605 ) ) ;
#20735 = CARTESIAN_POINT ( 'NONE',  ( 1.989925793838051682, 17.03278999510542846, 0.1141983552420977044 ) ) ;
#20736 = DIRECTION ( 'NONE',  ( 0.000000000000000000, -1.000000000000000000, -0.000000000000000000 ) ) ;
#20737 = CARTESIAN_POINT ( 'NONE',  ( 53.84486179190094646, -76.79125307200000350, -6.412645463410259872 ) ) ;
#20738 = DIRECTION ( 'NONE',  ( -0.8609107660235848503, 0.000000000000000000, 0.5087559856598096175 ) ) ;
#20739 = ORIENTED_EDGE ( 'NONE', *, *, #6125, .T. ) ;
#20740 = CARTESIAN_POINT ( 'NONE',  ( 54.11611804786240043, 32.54502000000000095, -30.58983753981140197 ) ) ;
#20741 = EDGE_CURVE ( 'NONE', #4404, #12549, #6962, .T. ) ;
#20742 = CARTESIAN_POINT ( 'NONE',  ( 21.58673283863862125, -3.402115365398042268, -14.98991958019304072 ) ) ;
#20744 = DIRECTION ( 'NONE',  ( 0.2490110332224869660, 9.093548366658288884E-16, -0.9685006480810788299 ) ) ;
#20743 = DIRECTION ( 'NONE',  ( -0.000000000000000000, -1.000000000000000000, 0.000000000000000000 ) ) ;
#20745 = ORIENTED_EDGE ( 'NONE', *, *, #1543, .T. ) ;
#20746 = EDGE_CURVE ( 'NONE', #17636, #10480, #18091, .T. ) ;
#20747 = ORIENTED_EDGE ( 'NONE', *, *, #5568, .F. ) ;
#20748 = EDGE_CURVE ( 'NONE', #8700, #15141, #3218, .T. ) ;
#20749 = CARTESIAN_POINT ( 'NONE',  ( 6.736797773167128689, 11.82549305421424179, 4.274780649399409604 ) ) ;
#20750 = AXIS2_PLACEMENT_3D ( 'NONE', #18363, #1771, #7087 ) ;
#20752 = DIRECTION ( 'NONE',  ( 0.8667647648559581031, 0.000000000000000000, 0.4987171968201974948 ) ) ;
#20751 = CARTESIAN_POINT ( 'NONE',  ( 1.503361638335910078, 12.54475284465800300, 8.020844464906803140 ) ) ;
#20753 = VERTEX_POINT ( 'NONE', #8726 ) ;
#20755 = CARTESIAN_POINT ( 'NONE',  ( 21.01748975371211259, -1.169157164984415465, -15.02132963540784694 ) ) ;
#20754 = CARTESIAN_POINT ( 'NONE',  ( 5.598399313467577798, 15.02198729771266272, 8.635687164693491624 ) ) ;
#20756 = EDGE_LOOP ( 'NONE', ( #1360, #2064, #8353, #8245, #11945, #16371 ) ) ;
#20757 = ORIENTED_EDGE ( 'NONE', *, *, #13005, .T. ) ;
#20758 = CARTESIAN_POINT ( 'NONE',  ( 7.757688011553915963, 12.41336384027103179, -0.1314292562850493673 ) ) ;
#20759 = ORIENTED_EDGE ( 'NONE', *, *, #12330, .F. ) ;
#20760 = AXIS2_PLACEMENT_3D ( 'NONE', #20470, #6789, #15326 ) ;
#20761 = CYLINDRICAL_SURFACE ( 'NONE', #3971, 0.7950200000000005041 ) ;
#20762 = LINE ( 'NONE', #5842, #16402 ) ;
#20763 = DIRECTION ( 'NONE',  ( 0.000000000000000000, -1.000000000000000000, -0.000000000000000000 ) ) ;
#20764 = DIRECTION ( 'NONE',  ( 0.000000000000000000, 1.000000000000000000, 0.000000000000000000 ) ) ;
#20765 = CARTESIAN_POINT ( 'NONE',  ( 3.332715841987694105, 18.44329026216701095, 8.753185752870537684 ) ) ;
#20766 = ORIENTED_EDGE ( 'NONE', *, *, #20741, .F. ) ;
#20767 = CARTESIAN_POINT ( 'NONE',  ( 0.3562249685988690961, 14.10021357005799025, 0.7816037492391179065 ) ) ;
#20768 = DIRECTION ( 'NONE',  ( -1.000000000000000000, 0.000000000000000000, 0.000000000000000000 ) ) ;
#20769 = DIRECTION ( 'NONE',  ( 0.2490110332224850231, 0.000000000000000000, -0.9685006480810791629 ) ) ;
#20770 = FACE_BOUND ( 'NONE', #9335, .T. ) ;
#20771 = ORIENTED_EDGE ( 'NONE', *, *, #7225, .F. ) ;
#20772 = EDGE_CURVE ( 'NONE', #21204, #21133, #6632, .T. ) ;
#20773 = EDGE_LOOP ( 'NONE', ( #12426, #17918, #21009, #741 ) ) ;
#20774 = CARTESIAN_POINT ( 'NONE',  ( 10.67274365531825886, 12.31998346384714083, 5.733264041280263790 ) ) ;
#20775 = DIRECTION ( 'NONE',  ( 0.4080888115384288528, 0.000000000000000000, 0.9129422336036122632 ) ) ;
#20776 = CARTESIAN_POINT ( 'NONE',  ( 11.48387577411441995, 11.17105998287007118, -1.405223482900355370 ) ) ;
#20777 = ORIENTED_EDGE ( 'NONE', *, *, #19924, .F. ) ;
#20778 = EDGE_LOOP ( 'NONE', ( #6048, #1690, #15030, #863 ) ) ;
#20779 = CARTESIAN_POINT ( 'NONE',  ( -51.02421882195815783, -5.714364999999999029, -23.02637480153789795 ) ) ;
#20780 = CIRCLE ( 'NONE', #19012, 30.16249999999999076 ) ;
#20781 = CARTESIAN_POINT ( 'NONE',  ( 7.363730569273300830, 17.62799059285756798, -2.758751801371228662 ) ) ;
#20782 = CARTESIAN_POINT ( 'NONE',  ( 7.274658096226261250, 13.47081914689558069, 6.777003322798922369 ) ) ;
#20783 = CARTESIAN_POINT ( 'NONE',  ( 8.781357490942916399, -6.752907499999998286, -18.85455479843708559 ) ) ;
#20784 = B_SPLINE_CURVE_WITH_KNOTS ( 'NONE', 3,
 ( #11471, #4837, #15127, #1508 ),
 .UNSPECIFIED., .F., .F.,
 ( 4, 4 ),
 ( 0.008535883516945940233, 0.009146310752443962550 ),
 .UNSPECIFIED. ) ;
#20785 = CARTESIAN_POINT ( 'NONE',  ( 5.955397547760478361, 12.33419677638291745, 0.8607368628538174526 ) ) ;
#20786 = CARTESIAN_POINT ( 'NONE',  ( 7.257706657338564682, 13.79373289338204600, 6.896359763853915581 ) ) ;
#20787 = DIRECTION ( 'NONE',  ( 0.000000000000000000, 1.000000000000000000, 0.000000000000000000 ) ) ;
#20788 = CARTESIAN_POINT ( 'NONE',  ( 13.41334640871851036, 18.63767531088674190, 6.295207162212891561 ) ) ;
#20789 = CARTESIAN_POINT ( 'NONE',  ( 7.505451342482677646, 16.64385683817606321, 8.498745805386123564 ) ) ;
#20790 = LINE ( 'NONE', #15749, #15307 ) ;
#20791 = CARTESIAN_POINT ( 'NONE',  ( 26.59062499999999929, 1.984375000000000000, 8.731249999999999289 ) ) ;
#20792 = CARTESIAN_POINT ( 'NONE',  ( 0.1787847043407926884, 13.13615472609876100, 2.181548182976034145 ) ) ;
#20793 = CARTESIAN_POINT ( 'NONE',  ( -23.34164412188400561, 41.43438499999999891, -25.36579984571316615 ) ) ;
#20794 = LINE ( 'NONE', #4341, #6055 ) ;
#20795 = CARTESIAN_POINT ( 'NONE',  ( 17.76390347290949379, 1.904479906339193507, -14.93461845486462458 ) ) ;
#20796 = LINE ( 'NONE', #17399, #9218 ) ;
#20797 = EDGE_CURVE ( 'NONE', #20661, #1499, #9955, .T. ) ;
#20798 = AXIS2_PLACEMENT_3D ( 'NONE', #18625, #11896, #8251 ) ;
#20799 = CARTESIAN_POINT ( 'NONE',  ( 10.14679030185686592, 10.59407055638359196, 1.519975852731572541 ) ) ;
#20800 = VERTEX_POINT ( 'NONE', #18571 ) ;
#20801 = DIRECTION ( 'NONE',  ( -0.8558687090795832342, 0.000000000000000000, 0.5171931484643309540 ) ) ;
#20802 = CARTESIAN_POINT ( 'NONE',  ( 11.89704164873937842, 11.32715860939759267, 0.2885734480728872620 ) ) ;
#20803 = CARTESIAN_POINT ( 'NONE',  ( 6.051356052310012501, 11.21701599786416104, 1.395022787371462236 ) ) ;
#20804 = DIRECTION ( 'NONE',  ( 0.000000000000000000, -1.000000000000000000, 0.000000000000000000 ) ) ;
#20805 = ORIENTED_EDGE ( 'NONE', *, *, #6584, .F. ) ;
#20806 = PRODUCT_CONTEXT ( 'NONE', #9318, 'mechanical' ) ;
#20807 = PLANE ( 'NONE',  #2859 ) ;
#20808 = CARTESIAN_POINT ( 'NONE',  ( 52.49113927203492125, -5.166360000000002728, -16.14695822742135078 ) ) ;
#20809 = MANIFOLD_SOLID_BREP ( 'Stock-MAS-676-1', #40 ) ;
#20810 = CARTESIAN_POINT ( 'NONE',  ( 14.16117470977285109, -8.465632521890594120, -16.45114775117519912 ) ) ;
#20811 = ORIENTED_EDGE ( 'NONE', *, *, #7352, .T. ) ;
#20812 = CARTESIAN_POINT ( 'NONE',  ( 9.653377856726027773, 12.37763185624888074, -1.110883424812121767 ) ) ;
#20813 = CARTESIAN_POINT ( 'NONE',  ( 4.101486013225753346, 20.36808788457486585, 5.283137556898260812 ) ) ;
#20814 = AXIS2_PLACEMENT_3D ( 'NONE', #13074, #18031, #19464 ) ;
#20815 = CARTESIAN_POINT ( 'NONE',  ( 12.91387984719911586, 18.46447794879854243, 6.063291446324524436 ) ) ;
#20816 = DIRECTION ( 'NONE',  ( -0.7334850928793772429, 0.6768732144311025989, 0.06198604769976985562 ) ) ;
#20817 = CARTESIAN_POINT ( 'NONE',  ( 9.256853431388732290, -1.983739999999999393, -17.09316853730597074 ) ) ;
#20818 = CARTESIAN_POINT ( 'NONE',  ( 19.71042948723761867, -2.147631015047439362, -14.24545724219409770 ) ) ;
#20819 = CARTESIAN_POINT ( 'NONE',  ( 30.41963056417667488, -1.983739999999999837, -8.653862521447852174 ) ) ;
#20820 = EDGE_CURVE ( 'NONE', #14694, #10716, #5292, .T. ) ;
#20821 = COLOUR_RGB ( '', 0.72549020, 0.75294118, 0.79215686) ;
#20822 = ORIENTED_EDGE ( 'NONE', *, *, #10471, .F. ) ;
#20823 = EDGE_CURVE ( 'NONE', #624, #288, #13796, .T. ) ;
#20824 = CARTESIAN_POINT ( 'NONE',  ( 13.11485487186891241, 18.81117101484460363, 6.766740726881102397 ) ) ;
#20825 = CARTESIAN_POINT ( 'NONE',  ( 52.86938555161624009, 40.05505435406290360, -16.95752595126053919 ) ) ;
#20826 = ORIENTED_EDGE ( 'NONE', *, *, #13219, .F. ) ;
#20827 = CARTESIAN_POINT ( 'NONE',  ( 10.10221342230659758, 11.41795989899646280, 1.305658110966970709 ) ) ;
#20828 = CARTESIAN_POINT ( 'NONE',  ( -0.8970842057359728061, -1.594802499999999013, -22.54358764576276286 ) ) ;
#20829 = CYLINDRICAL_SURFACE ( 'NONE', #11742, 1.984375000000000000 ) ;
#20830 = AXIS2_PLACEMENT_3D ( 'NONE', #15966, #20574, #15643 ) ;
#20832 = CARTESIAN_POINT ( 'NONE',  ( -51.69815163306579819, -5.714999999999999858, -7.436124251198355850 ) ) ;
#20831 = CARTESIAN_POINT ( 'NONE',  ( 3.174975191938078645, 15.51072843360936204, -0.9428492389082121505 ) ) ;
#20833 = VERTEX_POINT ( 'NONE', #20658 ) ;
#20834 =( NAMED_UNIT ( * ) PLANE_ANGLE_UNIT ( ) SI_UNIT ( $, .RADIAN. ) );
#20835 = CARTESIAN_POINT ( 'NONE',  ( 1.406764971174492729, 9.129395000000000593, 8.660233583965718296 ) ) ;
#20836 = ORIENTED_EDGE ( 'NONE', *, *, #16446, .F. ) ;
#20837 = CARTESIAN_POINT ( 'NONE',  ( 29.19635173153840313, 32.54502000000000095, -6.218966092919240296 ) ) ;
#20838 = AXIS2_PLACEMENT_3D ( 'NONE', #4053, #96, #1864 ) ;
#20839 = CARTESIAN_POINT ( 'NONE',  ( 17.23303716620361214, -7.327103372956576877, -15.95966167909989508 ) ) ;
#20840 = ORIENTED_EDGE ( 'NONE', *, *, #16168, .T. ) ;
#20841 = LINE ( 'NONE', #847, #8907 ) ;
#20842 = EDGE_CURVE ( 'NONE', #1054, #17145, #12446, .T. ) ;
#20843 = CARTESIAN_POINT ( 'NONE',  ( 12.72410813526706264, 20.52725722417916288, 5.592342314984960261 ) ) ;
#20844 = AXIS2_PLACEMENT_3D ( 'NONE', #15024, #10125, #172 ) ;
#20845 = CARTESIAN_POINT ( 'NONE',  ( 46.03750000000000142, 0.000000000000000000, -10.31874999999999964 ) ) ;
#20846 = LINE ( 'NONE', #1061, #10500 ) ;
#20847 = ORIENTED_EDGE ( 'NONE', *, *, #964, .F. ) ;
#20848 = ADVANCED_FACE ( 'NONE', ( #14284 ), #2433, .T. ) ;
#20849 = CARTESIAN_POINT ( 'NONE',  ( 20.23508736156870569, -1.359449706705495364, -14.75410053729980397 ) ) ;
#20850 = CARTESIAN_POINT ( 'NONE',  ( 13.28822531734660828, -1.983739999999999393, -15.23578611614444078 ) ) ;
#20851 = CARTESIAN_POINT ( 'NONE',  ( 17.55504807725674965, -8.549671308339609865, -15.78569734679938996 ) ) ;
#20853 = DIRECTION ( 'NONE',  ( 0.000000000000000000, -1.000000000000000000, 0.000000000000000000 ) ) ;
#20852 = CARTESIAN_POINT ( 'NONE',  ( 44.27024749654656688, -9.531985000000000596, -8.722764363618033201 ) ) ;
#20854 = VECTOR ( 'NONE', #8546, 1000.000000000000000 ) ;
#20855 = VERTEX_POINT ( 'NONE', #4197 ) ;
#20856 = ORIENTED_EDGE ( 'NONE', *, *, #2974, .F. ) ;
#20857 = AXIS2_PLACEMENT_3D ( 'NONE', #53, #13455, #7110 ) ;
#20859 = CARTESIAN_POINT ( 'NONE',  ( 59.61686353177688602, 36.51313500000000545, -0.7993558564620834028 ) ) ;
#20858 = CARTESIAN_POINT ( 'NONE',  ( 3.499273979999799611, 15.44861990895924819, -1.457855545221536042 ) ) ;
#20860 = VECTOR ( 'NONE', #19739, 1000.000000000000000 ) ;
#20861 = VERTEX_POINT ( 'NONE', #17690 ) ;
#20862 = CARTESIAN_POINT ( 'NONE',  ( 5.571606759789074381, 16.20829462093140094, 8.802327946292905381 ) ) ;
#20863 = VERTEX_POINT ( 'NONE', #15610 ) ;
#20864 = ORIENTED_EDGE ( 'NONE', *, *, #8550, .T. ) ;
#20865 = ORIENTED_EDGE ( 'NONE', *, *, #5593, .F. ) ;
#20866 = CARTESIAN_POINT ( 'NONE',  ( 3.179812809151942421, 12.83994299369714653, 6.696510645369547099 ) ) ;
#20867 = EDGE_CURVE ( 'NONE', #18768, #4510, #2091, .T. ) ;
#20868 = AXIS2_PLACEMENT_3D ( 'NONE', #10866, #16403, #14752 ) ;
#20869 = ADVANCED_FACE ( 'NONE', ( #5409 ), #2318, .F. ) ;
#20870 = EDGE_CURVE ( 'NONE', #1216, #17975, #11723, .T. ) ;
#20871 = VECTOR ( 'NONE', #18161, 1000.000000000000114 ) ;
#20872 = CARTESIAN_POINT ( 'NONE',  ( 2.318742500528585104, 0.02198808074787805128, 9.037480505500679939 ) ) ;
#20873 = DIRECTION ( 'NONE',  ( 0.9636276526537417286, 0.000000000000000000, -0.2672484743474499158 ) ) ;
#20874 = DIRECTION ( 'NONE',  ( 0.9685006480810793850, 0.000000000000000000, 0.2490110332224848011 ) ) ;
#20875 = CARTESIAN_POINT ( 'NONE',  ( 2.268027742546366632, 20.95393721777114138, 6.068657805862470056 ) ) ;
#20876 = VECTOR ( 'NONE', #6630, 1000.000000000000000 ) ;
#20877 = VERTEX_POINT ( 'NONE', #21002 ) ;
#20878 = CARTESIAN_POINT ( 'NONE',  ( 4.845298251511239940, 19.94879251081626137, 6.357549859093562183 ) ) ;
#20879 = DIRECTION ( 'NONE',  ( 0.000000000000000000, 1.000000000000000000, 0.000000000000000000 ) ) ;
#20880 = CARTESIAN_POINT ( 'NONE',  ( 13.00897473812072391, 21.65922317907614314, 1.991038036765448327 ) ) ;
#20881 = CARTESIAN_POINT ( 'NONE',  ( 65.90927232300019512, 0.000000000000000000, -13.30734117861468135 ) ) ;
#20882 = VERTEX_POINT ( 'NONE', #15728 ) ;
#20883 = ORIENTED_EDGE ( 'NONE', *, *, #8174, .T. ) ;
#20884 = CARTESIAN_POINT ( 'NONE',  ( 8.839373267820224811, 17.29611120545237313, -3.150632400723435200 ) ) ;
#20885 =( BOUNDED_CURVE ( )  B_SPLINE_CURVE ( 3, ( #8313, #20336, #11961, #12626 ),
 .UNSPECIFIED., .F., .T. ) 
 B_SPLINE_CURVE_WITH_KNOTS ( ( 4, 4 ),
 ( 4.712488883238074244, 6.283478609653115221 ),
 .UNSPECIFIED. ) 
 CURVE ( )  GEOMETRIC_REPRESENTATION_ITEM ( )  RATIONAL_B_SPLINE_CURVE ( ( 1.000000000000000000, 0.8046922671927911885, 0.8046922671927911885, 1.000000000000000000 ) ) 
 REPRESENTATION_ITEM ( '' )  );
#20887 = FACE_OUTER_BOUND ( 'NONE', #12263, .T. ) ;
#20886 = CARTESIAN_POINT ( 'NONE',  ( -16.88621914012359326, -3.266559801243759331, -10.37804376527844141 ) ) ;
#20888 = CARTESIAN_POINT ( 'NONE',  ( 12.97938784431679871, 11.59103285605196376, 4.871812665424503308 ) ) ;
#20889 = ORIENTED_EDGE ( 'NONE', *, *, #21663, .T. ) ;
#20890 = AXIS2_PLACEMENT_3D ( 'NONE', #2857, #14711, #18000 ) ;
#20891 = VERTEX_POINT ( 'NONE', #20881 ) ;
#20892 = CARTESIAN_POINT ( 'NONE',  ( 38.28489021960990613, 38.88803500000000213, 2.732679409805250703 ) ) ;
#20893 = CIRCLE ( 'NONE', #13853, 0.7950199999999993938 ) ;
#20894 = AXIS2_PLACEMENT_3D ( 'NONE', #5075, #19884, #4756 ) ;
#20895 = CARTESIAN_POINT ( 'NONE',  ( 7.456794536360651371, 18.25628204104152630, -2.578069215391849411 ) ) ;
#20896 = CARTESIAN_POINT ( 'NONE',  ( 3.854910616174523241, 17.18874207142246391, -0.6971550151776942927 ) ) ;
#20897 = DIRECTION ( 'NONE',  ( 0.7334850928793760216, 0.6768732144311038201, -0.06198604769976983481 ) ) ;
#20898 = CARTESIAN_POINT ( 'NONE',  ( 5.752222213375247861, 13.13460201027072216, -0.1270116662948033992 ) ) ;
#20899 = AXIS2_PLACEMENT_3D ( 'NONE', #14036, #12360, #15370 ) ;
#20900 = VECTOR ( 'NONE', #18785, 1000.000000000000227 ) ;
#20901 = CARTESIAN_POINT ( 'NONE',  ( 2.363086814207483677, 20.01344514090250826, 6.254446941780233971 ) ) ;
#20902 = DIRECTION ( 'NONE',  ( 0.000000000000000000, 1.000000000000000000, 0.000000000000000000 ) ) ;
#20903 = EDGE_CURVE ( 'NONE', #7959, #3770, #4330, .T. ) ;
#20904 = EDGE_CURVE ( 'NONE', #2298, #3111, #18777, .T. ) ;
#20905 = CARTESIAN_POINT ( 'NONE',  ( 13.59138924169983653, 12.98021359793846230, 5.706136380332087477 ) ) ;
#20906 = CARTESIAN_POINT ( 'NONE',  ( 4.597578589995645615, 11.87873374808372162, 3.870235249179852399 ) ) ;
#20907 = APPLICATION_CONTEXT ( 'automotive_design' ) ;
#20908 = CIRCLE ( 'NONE', #5373, 0.7950199999999993938 ) ;
#20909 = DIRECTION ( 'NONE',  ( 0.6702301885068632226, 0.000000000000000000, 0.7421532822901576454 ) ) ;
#20910 = DIRECTION ( 'NONE',  ( 0.000000000000000000, 1.000000000000000000, 0.000000000000000000 ) ) ;
#20911 = CARTESIAN_POINT ( 'NONE',  ( 5.463696641192596459, 17.51037618698124376, 8.782383522816124000 ) ) ;
#20912 = CARTESIAN_POINT ( 'NONE',  ( 1.309911988839522756, 18.71936051987669103, 9.004577120499568821 ) ) ;
#20913 = CARTESIAN_POINT ( 'NONE',  ( 57.23009918853844624, 34.52875999999999834, -20.42665903041912401 ) ) ;
#20914 = CARTESIAN_POINT ( 'NONE',  ( 2.488260037450269913, 12.01182523388594170, 3.580977260526816863 ) ) ;
#20915 = CARTESIAN_POINT ( 'NONE',  ( 1.268730000000000135, 8.334374999999999645, -88.70972349879099283 ) ) ;
#20916 = PLANE ( 'NONE',  #6409 ) ;
#20917 = CARTESIAN_POINT ( 'NONE',  ( 11.56302892044394248, -0.1067246172791157244, -16.79663542313268465 ) ) ;
#20918 = ORIENTED_EDGE ( 'NONE', *, *, #10124, .T. ) ;
#20919 = DIRECTION ( 'NONE',  ( 0.000000000000000000, 1.000000000000000000, 0.000000000000000000 ) ) ;
#20920 = AXIS2_PLACEMENT_3D ( 'NONE', #8425, #4902, #20139 ) ;
#20921 = PRESENTATION_LAYER_ASSIGNMENT (  '', '', ( #11042 ) ) ;
#20922 = CARTESIAN_POINT ( 'NONE',  ( 59.61686353177688602, 34.52875999999999834, -0.7993558564620834028 ) ) ;
#20923 = CARTESIAN_POINT ( 'NONE',  ( 11.14095035894017016, 12.07673251640017575, 5.753578539164537986 ) ) ;
#20924 = EDGE_LOOP ( 'NONE', ( #4863, #1095 ) ) ;
#20925 = DIRECTION ( 'NONE',  ( -0.9959941601142525691, 0.000000000000000000, -0.08941830359777946935 ) ) ;
#20926 = CARTESIAN_POINT ( 'NONE',  ( 11.16894477032718669, 14.35577606251322536, -3.188208178424544403 ) ) ;
#20927 = CARTESIAN_POINT ( 'NONE',  ( 5.551670149194028347, 17.88589146158793497, -1.957965570236789521 ) ) ;
#20928 = CARTESIAN_POINT ( 'NONE',  ( 49.28028498622276032, 32.54502000000000095, -25.68670502218146368 ) ) ;
#20929 = CARTESIAN_POINT ( 'NONE',  ( 2.748346265335036342, 12.03771362664550182, 5.108134015972813913 ) ) ;
#20930 = ORIENTED_EDGE ( 'NONE', *, *, #13217, .T. ) ;
#20931 = ITEM_DEFINED_TRANSFORMATION ( 'NONE', 'NONE', #13725,  #2234 ) ;
#20932 = DIRECTION ( 'NONE',  ( 0.000000000000000000, 1.000000000000000000, 0.000000000000000000 ) ) ;
#20933 = VECTOR ( 'NONE', #9810, 1000.000000000000000 ) ;
#20934 = CARTESIAN_POINT ( 'NONE',  ( 5.079859231761485461, 20.56621614536522458, 2.293009940660624135 ) ) ;
#20935 = CARTESIAN_POINT ( 'NONE',  ( -6.100806958593727458, -1.594802499992218126, -35.21050882107348912 ) ) ;
#20936 = ADVANCED_FACE ( 'NONE', ( #3987 ), #7300, .F. ) ;
#20937 = ORIENTED_EDGE ( 'NONE', *, *, #10760, .F. ) ;
#20938 = CIRCLE ( 'NONE', #9634, 3.175000000000000711 ) ;
#20939 = CARTESIAN_POINT ( 'NONE',  ( 12.89342041094828950, 11.95028677413862184, 4.185046594104111506 ) ) ;
#20940 = CARTESIAN_POINT ( 'NONE',  ( 13.22309003533597149, 14.87475635823169640, 6.306761496560224778 ) ) ;
#20941 = DIRECTION ( 'NONE',  ( 0.8334497143791951279, 0.000000000000000000, 0.5525953072558960066 ) ) ;
#20942 = CARTESIAN_POINT ( 'NONE',  ( 1.961280780403269919, 14.65425108942523558, -0.5112595838893696509 ) ) ;
#20943 = DIRECTION ( 'NONE',  ( 0.08420877549337302259, 0.000000000000000000, 0.9964481331860212121 ) ) ;
#20944 = DIRECTION ( 'NONE',  ( -0.2490110332224855227, 0.000000000000000000, 0.9685006480810791629 ) ) ;
#20945 = CARTESIAN_POINT ( 'NONE',  ( 5.126637874363053626, 19.15177079234708657, 7.986558305953045611 ) ) ;
#20946 = AXIS2_PLACEMENT_3D ( 'NONE', #7598, #16233, #14585 ) ;
#20947 = CARTESIAN_POINT ( 'NONE',  ( 14.81518831363163358, 0.9547697385890643318, -15.81862495919960487 ) ) ;
#20948 = UNCERTAINTY_MEASURE_WITH_UNIT (LENGTH_MEASURE( 1.000000000000000082E-05 ), #3435, 'distance_accuracy_value', 'NONE');
#20949 = DIRECTION ( 'NONE',  ( 0.000000000000000000, 1.000000000000000000, 0.000000000000000000 ) ) ;
#20950 = ORIENTED_EDGE ( 'NONE', *, *, #190, .F. ) ;
#20951 = CARTESIAN_POINT ( 'NONE',  ( 11.88288295434202624, 10.32531656698114020, 0.6793906613759156388 ) ) ;
#20952 = CARTESIAN_POINT ( 'NONE',  ( -14.35397337327049172, 33.73373999999999739, -0.6462872510839714479 ) ) ;
#20953 = ORIENTED_EDGE ( 'NONE', *, *, #13437, .T. ) ;
#20954 = CARTESIAN_POINT ( 'NONE',  ( 9.294500025656509123, 15.45828556898034734, -2.774045182040303370 ) ) ;
#20955 = AXIS2_PLACEMENT_3D ( 'NONE', #14924, #11688, #8260 ) ;
#20956 = CARTESIAN_POINT ( 'NONE',  ( 0.9543875819854121811, 18.83975182281294636, 7.997141017239727923 ) ) ;
#20958 = PLANE ( 'NONE',  #2523 ) ;
#20957 = CARTESIAN_POINT ( 'NONE',  ( 0.6905276204882465629, 12.01664638779708127, 6.542292752354295082 ) ) ;
#20959 = ORIENTED_EDGE ( 'NONE', *, *, #9073, .F. ) ;
#20960 = CARTESIAN_POINT ( 'NONE',  ( -7.949728765565600597, 33.32892749999999893, -34.47798802950714503 ) ) ;
#20961 = CARTESIAN_POINT ( 'NONE',  ( 1.776310917873034523, 8.950320134663451555, 8.723978618964752130 ) ) ;
#20962 = ORIENTED_EDGE ( 'NONE', *, *, #7376, .F. ) ;
#20963 = CARTESIAN_POINT ( 'NONE',  ( 19.37805486502776375, 0.2182193654363457358, -15.04364546347907172 ) ) ;
#20964 = AXIS2_PLACEMENT_3D ( 'NONE', #3425, #21669, #1546 ) ;
#20965 = EDGE_CURVE ( 'NONE', #15944, #8589, #14064, .T. ) ;
#20966 = CARTESIAN_POINT ( 'NONE',  ( 17.35374163439162132, -7.465977657333252360, -16.26709871504590410 ) ) ;
#20967 = ORIENTED_EDGE ( 'NONE', *, *, #16898, .T. ) ;
#20968 = DIRECTION ( 'NONE',  ( 0.5087559856598092844, 0.000000000000000000, 0.8609107660235849613 ) ) ;
#20969 = CARTESIAN_POINT ( 'NONE',  ( 1.880748080628404706, 15.39144081427376420, 0.1755720974858563377 ) ) ;
#20970 = CARTESIAN_POINT ( 'NONE',  ( 20.92131311655350245, -1.145359114192535888, -15.19233952661473097 ) ) ;
#20971 = VECTOR ( 'NONE', #1111, 1000.000000000000227 ) ;
#20972 = DIRECTION ( 'NONE',  ( 0.000000000000000000, -1.000000000000000000, 0.000000000000000000 ) ) ;
#20973 = CYLINDRICAL_SURFACE ( 'NONE', #253, 9.524999999999998579 ) ;
#20974 = ORIENTED_EDGE ( 'NONE', *, *, #18022, .F. ) ;
#20975 = LINE ( 'NONE', #8799, #5070 ) ;
#20976 = LINE ( 'NONE', #2294, #3813 ) ;
#20977 = ORIENTED_EDGE ( 'NONE', *, *, #289, .F. ) ;
#20978 = ORIENTED_EDGE ( 'NONE', *, *, #5007, .T. ) ;
#20980 = DIRECTION ( 'NONE',  ( 0.000000000000000000, 1.000000000000000000, 0.000000000000000000 ) ) ;
#20979 = CARTESIAN_POINT ( 'NONE',  ( 1.494606009698838944, 12.54422677008150089, 8.023943171028003363 ) ) ;
#20981 = ORIENTED_EDGE ( 'NONE', *, *, #4449, .F. ) ;
#20982 = CARTESIAN_POINT ( 'NONE',  ( 4.977942198378800143, 11.41917163132907120, 5.497878961665747077 ) ) ;
#20983 = ADVANCED_FACE ( 'NONE', ( #20770, #17473 ), #19230, .T. ) ;
#20984 = VERTEX_POINT ( 'NONE', #5751 ) ;
#20985 = VERTEX_POINT ( 'NONE', #4090 ) ;
#20986 = VECTOR ( 'NONE', #6897, 1000.000000000000000 ) ;
#20987 = EDGE_CURVE ( 'NONE', #17151, #8453, #2559, .T. ) ;
#20988 = VERTEX_POINT ( 'NONE', #16050 ) ;
#20989 = EDGE_CURVE ( 'NONE', #20322, #11391, #15277, .T. ) ;
#20990 = EDGE_CURVE ( 'NONE', #1632, #14970, #14719, .T. ) ;
#20991 = AXIS2_PLACEMENT_3D ( 'NONE', #5943, #12600, #10931 ) ;
#20992 = B_SPLINE_CURVE_WITH_KNOTS ( 'NONE', 3,
 ( #9976, #21262, #11527, #11204, #18268, #9537, #4572, #11312, #348, #12079 ),
 .UNSPECIFIED., .F., .F.,
 ( 4, 2, 2, 2, 4 ),
 ( 0.0008058748238304858612, 0.001281964470574262520, 0.001758054117318039178, 0.002234143764061815619, 0.002710233410805592495 ),
 .UNSPECIFIED. ) ;
#20993 = DIRECTION ( 'NONE',  ( 0.6702301885068632226, 0.000000000000000000, 0.7421532822901576454 ) ) ;
#20994 = CARTESIAN_POINT ( 'NONE',  ( 2.520748753591570690, 34.12394749999999988, -24.56335908395234924 ) ) ;
#20995 = DIRECTION ( 'NONE',  ( -0.9579671649362034858, 0.000000000000000000, 0.2868778675745010109 ) ) ;
#20996 = PLANE ( 'NONE',  #6528 ) ;
#20997 = CARTESIAN_POINT ( 'NONE',  ( 3.607082928935879895, 13.97555289970940073, 8.644940775583602743 ) ) ;
#20998 = ORIENTED_EDGE ( 'NONE', *, *, #20702, .T. ) ;
#20999 = CARTESIAN_POINT ( 'NONE',  ( 5.924761280269495778, 20.92139076675124443, 3.649616420326865285 ) ) ;
#21000 = CARTESIAN_POINT ( 'NONE',  ( 12.62386444219163373, 13.08957250000000094, -17.86660850434754266 ) ) ;
#21001 = LINE ( 'NONE', #12392, #431 ) ;
#21002 = CARTESIAN_POINT ( 'NONE',  ( 53.25483508941461963, 0.000000000000000000, -5.879799058943532941 ) ) ;
#21003 = ORIENTED_EDGE ( 'NONE', *, *, #19137, .F. ) ;
#21004 = ORIENTED_EDGE ( 'NONE', *, *, #19607, .F. ) ;
#21005 = CARTESIAN_POINT ( 'NONE',  ( 6.060151407706388937, 11.20245161629656039, 3.350174019466126474 ) ) ;
#21007 = FACE_OUTER_BOUND ( 'NONE', #7058, .T. ) ;
#21006 = CARTESIAN_POINT ( 'NONE',  ( 49.72033008250774344, 0.000000000000000000, -2.687827786179598277 ) ) ;
#21008 = CARTESIAN_POINT ( 'NONE',  ( 13.10951894981414867, 12.11001230185141786, 5.455309207400817151 ) ) ;
#21009 = ORIENTED_EDGE ( 'NONE', *, *, #18748, .T. ) ;
#21010 = EDGE_CURVE ( 'NONE', #10479, #20861, #16685, .T. ) ;
#21011 = ORIENTED_EDGE ( 'NONE', *, *, #7025, .T. ) ;
#21012 = DIRECTION ( 'NONE',  ( -0.2672484743474500268, 0.000000000000000000, -0.9636276526537417286 ) ) ;
#21013 = MANIFOLD_SOLID_BREP ( 'Stock-MAS-676-1', #12795 ) ;
#21014 = CARTESIAN_POINT ( 'NONE',  ( 7.261187168899082778, 16.54920457881469886, -2.885752199914386029 ) ) ;
#21015 = CARTESIAN_POINT ( 'NONE',  ( 5.078941371105551994, 20.64340025166658421, 2.206626728022376582 ) ) ;
#21016 = DIRECTION ( 'NONE',  ( 0.000000000000000000, -1.000000000000000000, -0.000000000000000000 ) ) ;
#21017 = CARTESIAN_POINT ( 'NONE',  ( 9.026273815804650269, 17.99597701874386857, 6.937175287538173585 ) ) ;
#21018 = EDGE_CURVE ( 'NONE', #13089, #11451, #4346, .T. ) ;
#21019 = LINE ( 'NONE', #2226, #14271 ) ;
#21020 = CARTESIAN_POINT ( 'NONE',  ( 9.566581944649177771, 16.63265789203856571, 8.068133590630180763 ) ) ;
#21021 = AXIS2_PLACEMENT_3D ( 'NONE', #10991, #17747, #13928 ) ;
#21022 = DIRECTION ( 'NONE',  ( 0.000000000000000000, 1.000000000000000000, 0.000000000000000000 ) ) ;
#21023 = CARTESIAN_POINT ( 'NONE',  ( 5.974525327850455092, 11.27374497607938331, 1.150844946209645281 ) ) ;
#21024 = CARTESIAN_POINT ( 'NONE',  ( 0.5711861650135396928, 20.53971507009796582, 7.163690434893576153 ) ) ;
#21025 = DIRECTION ( 'NONE',  ( 0.000000000000000000, 0.000000000000000000, 1.000000000000000000 ) ) ;
#21026 = CARTESIAN_POINT ( 'NONE',  ( 3.438407941595215789, 20.64378046205170136, 3.597508128396356586 ) ) ;
#21027 = CARTESIAN_POINT ( 'NONE',  ( 9.256853431388732290, 34.52875999999999834, -17.09316853730597074 ) ) ;
#21028 = DIRECTION ( 'NONE',  ( 0.000000000000000000, 1.000000000000000000, 0.000000000000000000 ) ) ;
#21029 = CARTESIAN_POINT ( 'NONE',  ( 11.72699871342261169, 0.1411900731644356866, -16.74345117411255401 ) ) ;
#21030 = EDGE_LOOP ( 'NONE', ( #8836, #21780, #6727, #4727 ) ) ;
#21031 = DIRECTION ( 'NONE',  ( 0.000000000000000000, 1.000000000000000000, 0.000000000000000000 ) ) ;
#21032 = CARTESIAN_POINT ( 'NONE',  ( 10.25539797921433305, 10.56827346328852180, 1.972515333481110966 ) ) ;
#21033 = ORIENTED_EDGE ( 'NONE', *, *, #8412, .F. ) ;
#21034 = EDGE_CURVE ( 'NONE', #14160, #9035, #3625, .T. ) ;
#21035 = DIRECTION ( 'NONE',  ( 0.000000000000000000, 1.000000000000000000, 0.000000000000000000 ) ) ;
#21036 = EDGE_CURVE ( 'NONE', #2302, #18035, #20192, .T. ) ;
#21037 = CARTESIAN_POINT ( 'NONE',  ( 12.23137370410826819, 20.73799744225223662, -1.222527140174004101 ) ) ;
#21038 = EDGE_CURVE ( 'NONE', #14138, #14787, #11262, .T. ) ;
#21039 = CARTESIAN_POINT ( 'NONE',  ( 5.904678845644677487, 11.49597437809906175, 0.7599978852366778836 ) ) ;
#21040 = CARTESIAN_POINT ( 'NONE',  ( 28.56548256563643662, -3.968114999999999615, -12.12873025803960658 ) ) ;
#21041 = ORIENTED_EDGE ( 'NONE', *, *, #10409, .F. ) ;
#21042 = CONTEXT_DEPENDENT_SHAPE_REPRESENTATION ( #4681, #5640 ) ;
#21043 = DIRECTION ( 'NONE',  ( 0.6702301885068630005, 0.000000000000000000, 0.7421532822901580895 ) ) ;
#21044 = VERTEX_POINT ( 'NONE', #18009 ) ;
#21045 = CARTESIAN_POINT ( 'NONE',  ( 7.035885886489748664, 20.81034843036036008, 1.590094180731808082 ) ) ;
#21046 = CARTESIAN_POINT ( 'NONE',  ( 11.04177093970491796, 12.61615142531242206, 5.335282712017707318 ) ) ;
#21047 = DIRECTION ( 'NONE',  ( 0.000000000000000000, -1.000000000000000000, -0.000000000000000000 ) ) ;
#21048 = CARTESIAN_POINT ( 'NONE',  ( 54.36523883999320361, 74.97070807199999365, -30.28170612544299800 ) ) ;
#21049 = DIRECTION ( 'NONE',  ( 0.000000000000000000, 1.000000000000000000, 0.000000000000000000 ) ) ;
#21050 = ORIENTED_EDGE ( 'NONE', *, *, #18858, .T. ) ;
#21051 = CARTESIAN_POINT ( 'NONE',  ( 6.686115959966646649, 11.04801462030960124, 4.499309094865339809 ) ) ;
#21052 = DIRECTION ( 'NONE',  ( 0.000000000000000000, 1.000000000000000000, 0.000000000000000000 ) ) ;
#21053 = ORIENTED_EDGE ( 'NONE', *, *, #3794, .T. ) ;
#21054 = ADVANCED_FACE ( 'NONE', ( #9383 ), #881, .T. ) ;
#21055 = CARTESIAN_POINT ( 'NONE',  ( 11.89814607795056567, 20.86867481596476281, 3.568910319330255820 ) ) ;
#21056 = LINE ( 'NONE', #13009, #11989 ) ;
#21057 = CARTESIAN_POINT ( 'NONE',  ( 0.2969748822967107071, 20.02444497997899120, 6.387532496747772015 ) ) ;
#21059 = CARTESIAN_POINT ( 'NONE',  ( -17.46249999999999858, 32.54247999999999763, 0.000000000000000000 ) ) ;
#21058 = CARTESIAN_POINT ( 'NONE',  ( -0.1087599157681504863, 18.79999059560985231, 1.111494402889351862 ) ) ;
#21060 = VERTEX_POINT ( 'NONE', #978 ) ;
#21061 = SHAPE_REPRESENTATION_RELATIONSHIP ( 'NONE' , 'NONE' ,  #11147, #1381 ) ;
#21062 = DIRECTION ( 'NONE',  ( 0.000000000000000000, -1.000000000000000000, -0.000000000000000000 ) ) ;
#21063 = CARTESIAN_POINT ( 'NONE',  ( 39.64154476330273269, -5.625436815413037195, -3.259749160125199108 ) ) ;
#21064 = ORIENTED_EDGE ( 'NONE', *, *, #3055, .F. ) ;
#21065 = DIRECTION ( 'NONE',  ( 0.000000000000000000, 1.000000000000000000, 0.000000000000000000 ) ) ;
#21066 = CARTESIAN_POINT ( 'NONE',  ( 12.33924171467970154, -0.5403633132482419388, -16.54107158940488986 ) ) ;
#21067 = ORIENTED_EDGE ( 'NONE', *, *, #9240, .F. ) ;
#21068 = CARTESIAN_POINT ( 'NONE',  ( 59.55063415577301811, -1.983739999999999837, -22.52230776719629191 ) ) ;
#21069 = DIRECTION ( 'NONE',  ( 0.000000000000000000, -1.000000000000000000, -0.000000000000000000 ) ) ;
#21070 = AXIS2_PLACEMENT_3D ( 'NONE', #8538, #16745, #16842 ) ;
#21071 = CARTESIAN_POINT ( 'NONE',  ( 61.83151161312219557, 0.000000000000000000, -0.3645647634491749334 ) ) ;
#21072 = ORIENTED_EDGE ( 'NONE', *, *, #2720, .F. ) ;
#21073 = CARTESIAN_POINT ( 'NONE',  ( 12.25799425556778388, 34.52875999999999834, 0.2069032437451798767 ) ) ;
#21075 = LINE ( 'NONE', #9134, #8035 ) ;
#21074 = DIRECTION ( 'NONE',  ( 0.000000000000000000, -1.000000000000000000, 0.000000000000000000 ) ) ;
#21076 = EDGE_LOOP ( 'NONE', ( #16855, #3661, #10328, #6170 ) ) ;
#21077 = EDGE_LOOP ( 'NONE', ( #17230, #6403, #21686, #10379 ) ) ;
#21078 = EDGE_CURVE ( 'NONE', #337, #6373, #5741, .T. ) ;
#21079 = CARTESIAN_POINT ( 'NONE',  ( 17.92763173077782923, -8.291096309418946930, -14.38181802688392175 ) ) ;
#21081 = FACE_OUTER_BOUND ( 'NONE', #9348, .T. ) ;
#21080 = CARTESIAN_POINT ( 'NONE',  ( 3.419644087157343471, 18.28285541323128172, 8.928697526465610323 ) ) ;
#21082 = ORIENTED_EDGE ( 'NONE', *, *, #10980, .F. ) ;
#21083 = CARTESIAN_POINT ( 'NONE',  ( 3.536909635595521184, 14.31338586005548130, -1.014190559432231797 ) ) ;
#21084 = ORIENTED_EDGE ( 'NONE', *, *, #573, .F. ) ;
#21085 = CIRCLE ( 'NONE', #20352, 5.357812499999999645 ) ;
#21086 = ORIENTED_EDGE ( 'NONE', *, *, #8951, .T. ) ;
#21087 = VERTEX_POINT ( 'NONE', #9601 ) ;
#21088 = CARTESIAN_POINT ( 'NONE',  ( 2.916021650325829828, 12.21811100267743733, 5.442930941693839841 ) ) ;
#21089 = ADVANCED_FACE ( 'NONE', ( #2618 ), #9238, .T. ) ;
#21090 = LINE ( 'NONE', #7511, #19810 ) ;
#21091 = CARTESIAN_POINT ( 'NONE',  ( 39.44501451162916084, 37.83287603509175767, -3.443458352271670631 ) ) ;
#21092 = LINE ( 'NONE', #18002, #17460 ) ;
#21093 = DIRECTION ( 'NONE',  ( 0.2490110332224850509, 0.000000000000000000, -0.9685006480810792739 ) ) ;
#21094 = CARTESIAN_POINT ( 'NONE',  ( 2.327109608273303820, 11.46633807340895217, 2.834091541352135479 ) ) ;
#21095 = ORIENTED_EDGE ( 'NONE', *, *, #21707, .F. ) ;
#21096 = CARTESIAN_POINT ( 'NONE',  ( 19.79515554403045741, 34.52875999999999834, -10.69562145279641996 ) ) ;
#21097 = FACE_OUTER_BOUND ( 'NONE', #10816, .T. ) ;
#21098 = DIRECTION ( 'NONE',  ( -0.9173788132826627972, 0.000000000000000000, 0.3980152169705239440 ) ) ;
#21099 = VERTEX_POINT ( 'NONE', #19075 ) ;
#21100 = EDGE_LOOP ( 'NONE', ( #1749, #4071, #7360, #15831, #5079 ) ) ;
#21101 = EDGE_CURVE ( 'NONE', #12400, #10833, #10329, .T. ) ;
#21102 = CARTESIAN_POINT ( 'NONE',  ( 7.758210749474673484, 11.08822532131044092, 1.918839297919416209 ) ) ;
#21103 = EDGE_CURVE ( 'NONE', #10784, #8462, #9615, .T. ) ;
#21105 = CARTESIAN_POINT ( 'NONE',  ( 13.52848780941367934, 19.04150370632758182, -20.24560135404512451 ) ) ;
#21104 = LINE ( 'NONE', #5955, #16493 ) ;
#21106 = CARTESIAN_POINT ( 'NONE',  ( 11.37417598588403855, 11.47492681191282138, -1.878663321889223248 ) ) ;
#21107 = VERTEX_POINT ( 'NONE', #4279 ) ;
#21108 = ORIENTED_EDGE ( 'NONE', *, *, #6110, .T. ) ;
#21109 = LINE ( 'NONE', #5761, #21203 ) ;
#21110 = CARTESIAN_POINT ( 'NONE',  ( 7.285362733318168971, 16.88496392601005169, -2.871492799055576306 ) ) ;
#21111 = CARTESIAN_POINT ( 'NONE',  ( 4.987365615438958066, 18.75973248553390604, 7.424326911423349884 ) ) ;
#21112 = LINE ( 'NONE', #9396, #8384 ) ;
#21113 = CARTESIAN_POINT ( 'NONE',  ( 8.577539078451785315, 19.63064409721748760, 5.907937441234182963 ) ) ;
#21114 = AXIS2_PLACEMENT_3D ( 'NONE', #20176, #16876, #1723 ) ;
#21115 = DIRECTION ( 'NONE',  ( 0.08420877549337300871, 0.000000000000000000, 0.9964481331860212121 ) ) ;
#21116 = CARTESIAN_POINT ( 'NONE',  ( -40.81626320044254896, 38.26001999999999725, 60.06868603633916592 ) ) ;
#21117 = CARTESIAN_POINT ( 'NONE',  ( 11.56363519470911072, 15.66465130118744398, 7.635224955696247484 ) ) ;
#21118 = EDGE_CURVE ( 'NONE', #13623, #9951, #13923, .T. ) ;
#21119 = DIRECTION ( 'NONE',  ( 0.000000000000000000, 1.000000000000000000, 0.000000000000000000 ) ) ;
#21120 = DIRECTION ( 'NONE',  ( -0.2868778675745010664, 0.000000000000000000, -0.9579671649362032637 ) ) ;
#21121 = CARTESIAN_POINT ( 'NONE',  ( 0.01692536528957819947, 12.52705325500010325, 1.673389856107192264 ) ) ;
#21122 = CARTESIAN_POINT ( 'NONE',  ( 1.619022443389374066, 16.88178287650320897, 9.587058323116350422 ) ) ;
#21123 = CARTESIAN_POINT ( 'NONE',  ( -1.345424459097947834, 12.30439499999999953, 2.648158502653860324 ) ) ;
#21124 = CARTESIAN_POINT ( 'NONE',  ( 6.658410181020286700, 19.52167825130506174, 6.491640720976068479 ) ) ;
#21125 = CARTESIAN_POINT ( 'NONE',  ( 53.10323493417986640, 40.07865999999999929, -16.70631907733998034 ) ) ;
#21126 = DIRECTION ( 'NONE',  ( -0.6702301885068632226, 0.000000000000000000, -0.7421532822901576454 ) ) ;
#21127 = CARTESIAN_POINT ( 'NONE',  ( 11.62205894965410913, -0.01747396230990239108, -16.77748880035451151 ) ) ;
#21128 = ORIENTED_EDGE ( 'NONE', *, *, #2516, .T. ) ;
#21129 = CARTESIAN_POINT ( 'NONE',  ( 55.81697695389291169, -3.968114999999999615, -11.14520323105768362 ) ) ;
#21130 = CIRCLE ( 'NONE', #14451, 0.5079999999999984528 ) ;
#21131 = EDGE_CURVE ( 'NONE', #7945, #2248, #5823, .T. ) ;
#21132 = CARTESIAN_POINT ( 'NONE',  ( 10.76973421761783634, 11.01165039305489124, 4.129500176367342235 ) ) ;
#21133 = VERTEX_POINT ( 'NONE', #2168 ) ;
#21134 = CARTESIAN_POINT ( 'NONE',  ( 22.60253186962359706, 0.7628563159022999640, 10.29585832510018051 ) ) ;
#21135 = CARTESIAN_POINT ( 'NONE',  ( 5.587485780822771808, 18.11784435417043682, -1.888017477237385000 ) ) ;
#21136 = LINE ( 'NONE', #21040, #11628 ) ;
#21137 = EDGE_LOOP ( 'NONE', ( #10442, #20883, #14942, #13200 ) ) ;
#21138 = VECTOR ( 'NONE', #812, 1000.000000000000000 ) ;
#21139 = DIRECTION ( 'NONE',  ( -0.000000000000000000, 1.000000000000000000, 0.000000000000000000 ) ) ;
#21140 = EDGE_CURVE ( 'NONE', #20877, #21393, #8911, .T. ) ;
#21141 = DIRECTION ( 'NONE',  ( -0.07875956036501312318, 0.000000000000000000, 0.9968936410927243807 ) ) ;
#21142 = CIRCLE ( 'NONE', #15172, 0.5080000000000001181 ) ;
#21143 = ORIENTED_EDGE ( 'NONE', *, *, #20215, .F. ) ;
#21144 = CARTESIAN_POINT ( 'NONE',  ( 9.565946762921560875, 16.58550361725992772, 7.310886168574319832 ) ) ;
#21145 = CARTESIAN_POINT ( 'NONE',  ( 5.207204373775217832, 17.45024786592896149, 7.901522660181242053 ) ) ;
#21146 = EDGE_CURVE ( 'NONE', #21099, #18734, #5026, .T. ) ;
#21147 = CARTESIAN_POINT ( 'NONE',  ( 8.652634833497350186, 19.63015825768726330, 6.037056894049368516 ) ) ;
#21148 = ADVANCED_FACE ( 'NONE', ( #15690 ), #7157, .T. ) ;
#21149 = CARTESIAN_POINT ( 'NONE',  ( 42.27821610176829381, -1.983739999999999837, 7.496956594510385763 ) ) ;
#21150 = EDGE_CURVE ( 'NONE', #367, #19423, #20841, .T. ) ;
#21151 = CARTESIAN_POINT ( 'NONE',  ( 53.67193531911993176, -7.278946903169048355, -16.01476742963361843 ) ) ;
#21152 = DIRECTION ( 'NONE',  ( 0.2868778675745011220, 0.000000000000000000, 0.9579671649362033747 ) ) ;
#21153 = CARTESIAN_POINT ( 'NONE',  ( 4.961560515085757572, 19.69663529535471014, 7.584757291997314077 ) ) ;
#21154 = FACE_OUTER_BOUND ( 'NONE', #914, .T. ) ;
#21155 = VERTEX_POINT ( 'NONE', #17442 ) ;
#21156 = CARTESIAN_POINT ( 'NONE',  ( 11.64611064670678964, -6.985072876733208425, -15.86009521399990518 ) ) ;
#21157 = DIRECTION ( 'NONE',  ( -0.2227372614607790735, 0.000000000000000000, -0.9748785115884710528 ) ) ;
#21158 = ORIENTED_EDGE ( 'NONE', *, *, #19425, .T. ) ;
#21159 = CARTESIAN_POINT ( 'NONE',  ( 9.599060309614154463, 18.43758607429610308, -2.436434164187765816 ) ) ;
#21160 = CARTESIAN_POINT ( 'NONE',  ( 46.03750000000000142, -1.983739999999999393, -10.31874999999999964 ) ) ;
#21161 = CARTESIAN_POINT ( 'NONE',  ( 0.4283631078011292947, 19.87700971128948524, 6.719787991462967014 ) ) ;
#21162 = CARTESIAN_POINT ( 'NONE',  ( 17.38991127515316393, -8.420206286881226632, -15.29446703135092633 ) ) ;
#21164 = CARTESIAN_POINT ( 'NONE',  ( 22.04181838752732148, 16.26393749999999727, 0.06645525512612464325 ) ) ;
#21163 = CARTESIAN_POINT ( 'NONE',  ( 3.143185894743523612, 14.84625823140281753, 8.814386136658805881 ) ) ;
#21165 = ORIENTED_EDGE ( 'NONE', *, *, #1487, .T. ) ;
#21166 = DIRECTION ( 'NONE',  ( 0.000000000000000000, 1.000000000000000000, 0.000000000000000000 ) ) ;
#21167 = FACE_OUTER_BOUND ( 'NONE', #20633, .T. ) ;
#21168 = ORIENTED_EDGE ( 'NONE', *, *, #17042, .T. ) ;
#21169 = AXIS2_PLACEMENT_3D ( 'NONE', #21715, #13330, #4703 ) ;
#21170 = CARTESIAN_POINT ( 'NONE',  ( 66.79943102505561114, -3.968114999999999615, -12.07331878313145168 ) ) ;
#21171 = AXIS2_PLACEMENT_3D ( 'NONE', #20564, #14193, #10956 ) ;
#21172 = CARTESIAN_POINT ( 'NONE',  ( 20.34285548276758604, -3.328947532601270964, -15.22298867112224485 ) ) ;
#21173 = ORIENTED_EDGE ( 'NONE', *, *, #11498, .T. ) ;
#21174 = CARTESIAN_POINT ( 'NONE',  ( 7.535583205468054935, 13.14768317755540039, -1.049594630872383361 ) ) ;
#21175 = LINE ( 'NONE', #6034, #12756 ) ;
#21176 = EDGE_CURVE ( 'NONE', #2599, #17559, #1848, .T. ) ;
#21177 = VECTOR ( 'NONE', #3691, 1000.000000000000114 ) ;
#21178 = CARTESIAN_POINT ( 'NONE',  ( -1.427050033073577806, 3.961447500000001565, -23.44038945102687066 ) ) ;
#21179 = EDGE_LOOP ( 'NONE', ( #7239, #6497, #18869, #3415 ) ) ;
#21180 = CIRCLE ( 'NONE', #18025, 6.350000000000002309 ) ;
#21181 = DIRECTION ( 'NONE',  ( -0.2064631973582987667, 0.000000000000000000, 0.9784543669157944601 ) ) ;
#21182 = CARTESIAN_POINT ( 'NONE',  ( 46.03750000000000142, -14.84248999999999974, -10.31874999999999964 ) ) ;
#21183 = VERTEX_POINT ( 'NONE', #517 ) ;
#21184 = ORIENTED_EDGE ( 'NONE', *, *, #14121, .T. ) ;
#21185 = DIRECTION ( 'NONE',  ( 1.000000000000000000, 0.000000000000000000, 0.000000000000000000 ) ) ;
#21187 = CARTESIAN_POINT ( 'NONE',  ( 46.03750000000000142, 34.52875999999999834, -10.31874999999999964 ) ) ;
#21186 = CARTESIAN_POINT ( 'NONE',  ( 2.899943480386378614, 11.23735775897588240, 5.220590930253522721 ) ) ;
#21188 = VERTEX_POINT ( 'NONE', #7269 ) ;
#21189 = CARTESIAN_POINT ( 'NONE',  ( 3.548261816934641377, 14.10662813518449710, -0.9291583932840015159 ) ) ;
#21190 = ORIENTED_EDGE ( 'NONE', *, *, #13314, .T. ) ;
#21191 = AXIS2_PLACEMENT_3D ( 'NONE', #10079, #123, #13408 ) ;
#21192 = ORIENTED_EDGE ( 'NONE', *, *, #19775, .F. ) ;
#21193 = CARTESIAN_POINT ( 'NONE',  ( 0.8456107407395869746, 12.23494454746245097, 5.237939145250719797 ) ) ;
#21194 = EDGE_LOOP ( 'NONE', ( #9583, #8628, #1662, #14921 ) ) ;
#21195 = VECTOR ( 'NONE', #5244, 1000.000000000000114 ) ;
#21196 = CIRCLE ( 'NONE', #20473, 4.961572499999999941 ) ;
#21197 = EDGE_CURVE ( 'NONE', #21087, #11237, #6793, .T. ) ;
#21198 = DIRECTION ( 'NONE',  ( 0.7421532822901572013, 0.000000000000000000, -0.6702301885068637777 ) ) ;
#21199 = CARTESIAN_POINT ( 'NONE',  ( 39.59538228781720903, 37.96603874921844124, -3.302459560555300655 ) ) ;
#21200 = DIRECTION ( 'NONE',  ( 0.000000000000000000, 1.000000000000000000, 0.000000000000000000 ) ) ;
#21201 = CYLINDRICAL_SURFACE ( 'NONE', #8299, 0.7950200000000005041 ) ;
#21202 = CARTESIAN_POINT ( 'NONE',  ( 3.244888726987362304, 11.99121938177022173, 6.831822597935710562 ) ) ;
#21203 = VECTOR ( 'NONE', #4103, 1000.000000000000114 ) ;
#21204 = VERTEX_POINT ( 'NONE', #3950 ) ;
#21205 = VECTOR ( 'NONE', #19637, 1000.000000000000000 ) ;
#21206 = PLANE ( 'NONE',  #11767 ) ;
#21207 = LINE ( 'NONE', #18007, #420 ) ;
#21208 = DIRECTION ( 'NONE',  ( -0.2868778675745011220, 0.000000000000000000, -0.9579671649362034858 ) ) ;
#21209 = DIRECTION ( 'NONE',  ( -0.8583349619704301325, 0.000000000000000000, 0.5130897514657842828 ) ) ;
#21210 = ORIENTED_EDGE ( 'NONE', *, *, #735, .T. ) ;
#21211 = VERTEX_POINT ( 'NONE', #2282 ) ;
#21212 = CARTESIAN_POINT ( 'NONE',  ( 8.815742426116205621, 21.23906099414256232, 1.844918515833101624 ) ) ;
#21214 = CARTESIAN_POINT ( 'NONE',  ( -47.86049599909252805, 41.43438499999999891, -23.29373766372935961 ) ) ;
#21213 = DIRECTION ( 'NONE',  ( 0.000000000000000000, 0.000000000000000000, 1.000000000000000000 ) ) ;
#21215 = CARTESIAN_POINT ( 'NONE',  ( 10.94810466157118256, 16.27247983235652384, -4.349187853150674243 ) ) ;
#21216 = VERTEX_POINT ( 'NONE', #9020 ) ;
#21217 = ORIENTED_EDGE ( 'NONE', *, *, #5424, .T. ) ;
#21218 = CYLINDRICAL_SURFACE ( 'NONE', #16628, 0.7950200000000022804 ) ;
#21219 = CARTESIAN_POINT ( 'NONE',  ( 7.224900101663735974, 14.64899027572959689, -2.626539992268202006 ) ) ;
#21220 = LINE ( 'NONE', #17822, #9099 ) ;
#21221 = CARTESIAN_POINT ( 'NONE',  ( 6.774608736861511993, 20.53452479865724456, 1.173560763751360980 ) ) ;
#21222 = VECTOR ( 'NONE', #17948, 1000.000000000000114 ) ;
#21223 = AXIS2_PLACEMENT_3D ( 'NONE', #205, #13711, #13823 ) ;
#21224 = VECTOR ( 'NONE', #7582, 1000.000000000000000 ) ;
#21225 = CARTESIAN_POINT ( 'NONE',  ( 59.90456643211351917, 32.54502000000000095, -2.926035437812116946 ) ) ;
#21226 = ADVANCED_FACE ( 'NONE', ( #15796 ), #14251, .T. ) ;
#21227 = AXIS2_PLACEMENT_3D ( 'NONE', #7198, #18895, #1983 ) ;
#21228 = CARTESIAN_POINT ( 'NONE',  ( 12.30760114933989868, 21.61111399576532222, 3.840915675052047007 ) ) ;
#21229 = CIRCLE ( 'NONE', #1459, 30.16249999999998721 ) ;
#21230 = CARTESIAN_POINT ( 'NONE',  ( 39.11079947626275555, 0.000000000000000000, -27.65534212225540500 ) ) ;
#21231 = DIRECTION ( 'NONE',  ( 1.000000000000000000, 0.000000000000000000, 0.000000000000000000 ) ) ;
#21232 = CYLINDRICAL_SURFACE ( 'NONE', #3529, 0.7950199999999985057 ) ;
#21233 = CARTESIAN_POINT ( 'NONE',  ( 6.822374228803519181, 20.09399725779506340, 7.039163523395035149 ) ) ;
#21234 = CARTESIAN_POINT ( 'NONE',  ( 0.7138079833445840627, 11.42373057883981247, 4.642704508746212433 ) ) ;
#21235 = CARTESIAN_POINT ( 'NONE',  ( 54.51779242482700027, 1.984375000000000000, -30.64740209392260084 ) ) ;
#21236 = CARTESIAN_POINT ( 'NONE',  ( 1.161278549730571763, 12.40032227216336125, 6.252213015588909961 ) ) ;
#21237 = DIRECTION ( 'NONE',  ( 0.000000000000000000, 1.000000000000000000, -0.000000000000000000 ) ) ;
#21238 = FACE_BOUND ( 'NONE', #7583, .T. ) ;
#21239 = CARTESIAN_POINT ( 'NONE',  ( 13.94526350254431080, -8.131198800652363445, -15.30999825101322820 ) ) ;
#21240 = CIRCLE ( 'NONE', #4302, 0.7950199999999988387 ) ;
#21241 = ORIENTED_EDGE ( 'NONE', *, *, #6206, .T. ) ;
#21242 = CARTESIAN_POINT ( 'NONE',  ( 17.79723720954694954, 34.52875999999999834, -14.07647485258271303 ) ) ;
#21243 = AXIS2_PLACEMENT_3D ( 'NONE', #2237, #9305, #19585 ) ;
#21244 = AXIS2_PLACEMENT_3D ( 'NONE', #5757, #7842, #14289 ) ;
#21245 = CARTESIAN_POINT ( 'NONE',  ( 10.38674899259666162, 10.59278501052695098, 2.519868619535428955 ) ) ;
#21246 = ORIENTED_EDGE ( 'NONE', *, *, #3995, .T. ) ;
#21247 = CARTESIAN_POINT ( 'NONE',  ( 24.76323281030605017, 0.9575987068668280200, 10.42990517843087872 ) ) ;
#21248 = CIRCLE ( 'NONE', #788, 0.7950200000000005041 ) ;
#21249 = CARTESIAN_POINT ( 'NONE',  ( 12.62152852634566003, 21.21270663461748285, -0.1788462545625037481 ) ) ;
#21250 = CARTESIAN_POINT ( 'NONE',  ( 5.470336632480330863, 17.23705307414203247, -2.093767104412924684 ) ) ;
#21251 = AXIS2_PLACEMENT_3D ( 'NONE', #2541, #5848, #3879 ) ;
#21252 = CARTESIAN_POINT ( 'NONE',  ( 59.80894853325292360, -6.356984999999999886, -16.70545285374888778 ) ) ;
#21253 = CARTESIAN_POINT ( 'NONE',  ( 1.325961175420450333, 20.33382539468342287, 3.515434316510341883 ) ) ;
#21254 = VERTEX_POINT ( 'NONE', #12470 ) ;
#21255 = EDGE_CURVE ( 'NONE', #3908, #6597, #10690, .T. ) ;
#21256 = CARTESIAN_POINT ( 'NONE',  ( 67.40134256979101224, 30.56064500000000095, -13.30734117861468135 ) ) ;
#21257 = AXIS2_PLACEMENT_3D ( 'NONE', #16988, #18636, #6928 ) ;
#21258 = AXIS2_PLACEMENT_3D ( 'NONE', #16582, #21208, #11157 ) ;
#21259 = EDGE_CURVE ( 'NONE', #12951, #180, #10802, .T. ) ;
#21260 = CARTESIAN_POINT ( 'NONE',  ( 12.34322936788867331, 20.88809130931168312, -1.203018507871442599 ) ) ;
#21261 = EDGE_CURVE ( 'NONE', #18192, #3590, #732, .T. ) ;
#21262 = CARTESIAN_POINT ( 'NONE',  ( 38.18512253410862911, -6.196245922951924889, -4.927479914652647786 ) ) ;
#21263 = LINE ( 'NONE', #19496, #10346 ) ;
#21264 = LINE ( 'NONE', #16518, #18174 ) ;
#21265 = CARTESIAN_POINT ( 'NONE',  ( 1.663439973261383820, -0.7997824999999986195, -22.73355581192510044 ) ) ;
#21266 = CARTESIAN_POINT ( 'NONE',  ( 21.23967064989561493, -3.382426365437452009, -15.02713005365007959 ) ) ;
#21267 = CARTESIAN_POINT ( 'NONE',  ( 65.51436440461340283, 0.000000000000000000, -12.87863775929475985 ) ) ;
#21268 = ORIENTED_EDGE ( 'NONE', *, *, #5199, .F. ) ;
#21269 = DIRECTION ( 'NONE',  ( 0.000000000000000000, 1.000000000000000000, 0.000000000000000000 ) ) ;
#21270 = DIRECTION ( 'NONE',  ( -0.2672484743474500268, 0.000000000000000000, -0.9636276526537417286 ) ) ;
#21271 = VECTOR ( 'NONE', #16623, 1000.000000000000114 ) ;
#21272 = ORIENTED_EDGE ( 'NONE', *, *, #18905, .F. ) ;
#21273 = CARTESIAN_POINT ( 'NONE',  ( 12.35123053909024904, 20.10583435259948715, 4.755396859769023266 ) ) ;
#21274 = CARTESIAN_POINT ( 'NONE',  ( -12.21686131739395798, -1.587500000000002132, -1.090609736204202429 ) ) ;
#21275 = CARTESIAN_POINT ( 'NONE',  ( 0.7583887236725060932, 19.33151544516331199, 7.535919219584821249 ) ) ;
#21276 = CARTESIAN_POINT ( 'NONE',  ( 20.45077234916881892, -6.011631478081029378, -13.76232490753369397 ) ) ;
#21278 = FACE_OUTER_BOUND ( 'NONE', #3124, .T. ) ;
#21277 = CARTESIAN_POINT ( 'NONE',  ( 1.201550318572446319, 14.26529943814340129, 8.588777914063905783 ) ) ;
#21279 = ORIENTED_EDGE ( 'NONE', *, *, #18927, .T. ) ;
#21280 = EDGE_CURVE ( 'NONE', #12822, #218, #18796, .T. ) ;
#21281 = CARTESIAN_POINT ( 'NONE',  ( -1.848761088705630051, 9.129395000000000593, 7.884515871828260636 ) ) ;
#21282 = CIRCLE ( 'NONE', #11756, 20.83593750000000000 ) ;
#21283 = CARTESIAN_POINT ( 'NONE',  ( 1.916925818690368377, 8.800110775149704523, 8.731250000000001066 ) ) ;
#21284 = ORIENTED_EDGE ( 'NONE', *, *, #3537, .T. ) ;
#21285 = AXIS2_PLACEMENT_3D ( 'NONE', #18694, #10304, #8741 ) ;
#21286 = DIRECTION ( 'NONE',  ( -9.174536502825477718E-16, 1.000000000000000000, -1.085629106648973872E-14 ) ) ;
#21287 = ORIENTED_EDGE ( 'NONE', *, *, #2872, .F. ) ;
#21288 = CARTESIAN_POINT ( 'NONE',  ( 9.089864963733731429, 21.15296384697220233, 1.773382899297284210 ) ) ;
#21289 = CARTESIAN_POINT ( 'NONE',  ( 9.352501096662308555, 12.85887757399174092, 6.957954859781140478 ) ) ;
#21290 = CYLINDRICAL_SURFACE ( 'NONE', #18601, 0.5080000000000000071 ) ;
#21291 = CIRCLE ( 'NONE', #19547, 0.3962400000000008138 ) ;
#21292 = AXIS2_PLACEMENT_3D ( 'NONE', #12634, #679, #5539 ) ;
#21293 = ORIENTED_EDGE ( 'NONE', *, *, #7611, .T. ) ;
#21294 = CARTESIAN_POINT ( 'NONE',  ( 49.41235866845560309, 1.984375000000000000, -26.78690084448080100 ) ) ;
#21295 = B_SPLINE_CURVE_WITH_KNOTS ( 'NONE', 3,
 ( #856, #7599, #20436, #15079 ),
 .UNSPECIFIED., .F., .F.,
 ( 4, 4 ),
 ( 0.008550247267032764359, 0.009162609743145760585 ),
 .UNSPECIFIED. ) ;
#21296 = EDGE_LOOP ( 'NONE', ( #9361, #19340, #20132, #3720 ) ) ;
#21297 = ORIENTED_EDGE ( 'NONE', *, *, #2262, .F. ) ;
#21298 = FACE_OUTER_BOUND ( 'NONE', #17351, .T. ) ;
#21300 = FACE_OUTER_BOUND ( 'NONE', #710, .T. ) ;
#21299 = CARTESIAN_POINT ( 'NONE',  ( 3.648839215576543893, 16.52268874363389628, 9.299509987714628778 ) ) ;
#21301 = ORIENTED_EDGE ( 'NONE', *, *, #20870, .T. ) ;
#21302 = CARTESIAN_POINT ( 'NONE',  ( 3.899173628609031717, 18.90516298583656152, -0.8066410379536314013 ) ) ;
#21303 = ADVANCED_FACE ( 'NONE', ( #21499 ), #4558, .T. ) ;
#21304 = VECTOR ( 'NONE', #10584, 1000.000000000000114 ) ;
#21305 = ORIENTED_EDGE ( 'NONE', *, *, #15466, .T. ) ;
#21306 = EDGE_CURVE ( 'NONE', #21868, #19865, #9966, .T. ) ;
#21307 = VERTEX_POINT ( 'NONE', #2592 ) ;
#21308 = CIRCLE ( 'NONE', #12862, 3.968750000000001776 ) ;
#21309 = EDGE_LOOP ( 'NONE', ( #8336, #5822, #10489, #14751 ) ) ;
#21310 = CARTESIAN_POINT ( 'NONE',  ( 2.651964239740473683, 13.08893749999999834, 5.873042593501262232 ) ) ;
#21311 = VECTOR ( 'NONE', #19323, 1000.000000000000000 ) ;
#21312 = CARTESIAN_POINT ( 'NONE',  ( 6.585898268469219552, 30.56064500000000095, 4.694966092919240275 ) ) ;
#21313 = CARTESIAN_POINT ( 'NONE',  ( 29.22749461619170219, 39.28268749999999443, -4.986088976786413163 ) ) ;
#21314 = CARTESIAN_POINT ( 'NONE',  ( 39.62791084302666178, -1.983739999999999837, -24.65774797299118859 ) ) ;
#21315 = CARTESIAN_POINT ( 'NONE',  ( 3.461646834230382996, 12.83219514639866077, 7.850548974203960917 ) ) ;
#21316 = ORIENTED_EDGE ( 'NONE', *, *, #18409, .T. ) ;
#21317 = CARTESIAN_POINT ( 'NONE',  ( -51.69815163306579819, 38.26001999999999725, -7.436124251198355850 ) ) ;
#21318 = DIRECTION ( 'NONE',  ( 0.000000000000000000, 1.000000000000000000, 0.000000000000000000 ) ) ;
#21319 = CARTESIAN_POINT ( 'NONE',  ( 49.41195815393805901, -9.531985000000000596, -1.411525001868561224 ) ) ;
#21320 = CARTESIAN_POINT ( 'NONE',  ( 57.35354854712898742, 32.54502000000000095, -21.22263945788050776 ) ) ;
#21321 = CYLINDRICAL_SURFACE ( 'NONE', #2443, 0.7950200000000005041 ) ;
#21322 = ORIENTED_EDGE ( 'NONE', *, *, #1772, .F. ) ;
#21323 = EDGE_LOOP ( 'NONE', ( #11095, #20431, #11682, #5845, #17885 ) ) ;
#21324 = CARTESIAN_POINT ( 'NONE',  ( 9.248416887644976825, 12.30663295771102383, -1.050148961336570652 ) ) ;
#21326 = CARTESIAN_POINT ( 'NONE',  ( -29.36874999999999858, 30.56064500000000095, 8.335010000000000474 ) ) ;
#21325 = CARTESIAN_POINT ( 'NONE',  ( 13.11799571124250363, 19.43957250000000059, -19.78847697788343396 ) ) ;
#21327 = AXIS2_PLACEMENT_3D ( 'NONE', #17900, #2748, #9482 ) ;
#21328 = CARTESIAN_POINT ( 'NONE',  ( 12.13422153915409396, 21.45254555255133155, -1.556433456872093890 ) ) ;
#21329 = ORIENTED_EDGE ( 'NONE', *, *, #11517, .T. ) ;
#21330 = EDGE_LOOP ( 'NONE', ( #4589, #7762, #14797, #8391 ) ) ;
#21331 = EDGE_CURVE ( 'NONE', #1698, #2302, #15879, .T. ) ;
#21332 = DIRECTION ( 'NONE',  ( 0.000000000000000000, 1.000000000000000000, 0.000000000000000000 ) ) ;
#21333 = CARTESIAN_POINT ( 'NONE',  ( 8.390788493197108622, 21.17394158998719433, -0.2334963480496760335 ) ) ;
#21334 = CARTESIAN_POINT ( 'NONE',  ( 7.295279368536716547, 20.90511879603792167, 2.551392718645653090 ) ) ;
#21335 = VECTOR ( 'NONE', #7347, 1000.000000000000114 ) ;
#21336 = AXIS2_PLACEMENT_3D ( 'NONE', #13016, #19523, #19721 ) ;
#21337 = CYLINDRICAL_SURFACE ( 'NONE', #14991, 1.190624999999999822 ) ;
#21338 = DIRECTION ( 'NONE',  ( -0.9636276526537417286, 0.000000000000000000, 0.2672484743474501934 ) ) ;
#21339 = CARTESIAN_POINT ( 'NONE',  ( 3.604122478219174752, 16.52265399103842825, 9.312174804150144425 ) ) ;
#21340 = CARTESIAN_POINT ( 'NONE',  ( 0.7629431678296610952, 11.42074363723537189, 4.856465998727349742 ) ) ;
#21341 = VERTEX_POINT ( 'NONE', #12658 ) ;
#21342 = CARTESIAN_POINT ( 'NONE',  ( 7.046384120664519024, 18.17920521194865913, 7.360324746534422147 ) ) ;
#21343 = DIRECTION ( 'NONE',  ( 0.000000000000000000, 1.000000000000000000, 0.000000000000000000 ) ) ;
#21344 = CARTESIAN_POINT ( 'NONE',  ( -15.27766260488554195, 34.52875999999999834, -26.04727837583638461 ) ) ;
#21345 = CARTESIAN_POINT ( 'NONE',  ( 11.39261545403312326, -6.154307413984438035, -15.84502314252291733 ) ) ;
#21346 = CIRCLE ( 'NONE', #5110, 5.357812499999999645 ) ;
#21347 = VERTEX_POINT ( 'NONE', #12322 ) ;
#21348 = CARTESIAN_POINT ( 'NONE',  ( 8.505511374756364873, -1.594802499999999013, -20.97439202360551747 ) ) ;
#21349 = CARTESIAN_POINT ( 'NONE',  ( 9.553597871840317168, 19.49545814391576926, -2.744787722736090618 ) ) ;
#21350 = ORIENTED_EDGE ( 'NONE', *, *, #18827, .T. ) ;
#21351 = CARTESIAN_POINT ( 'NONE',  ( 29.02375794721179858, 1.691909351835945152, 10.69422218668175972 ) ) ;
#21352 = EDGE_CURVE ( 'NONE', #14925, #16536, #18940, .T. ) ;
#21353 = CARTESIAN_POINT ( 'NONE',  ( 12.34524511935337543, 20.90878755461004346, -0.9203087109956159528 ) ) ;
#21354 = CARTESIAN_POINT ( 'NONE',  ( 7.827212224107905847, 21.58676227676403059, 4.002251945881059925 ) ) ;
#21355 = CARTESIAN_POINT ( 'NONE',  ( -29.36874999999999858, 32.54502000000000095, 8.731885000000000119 ) ) ;
#21356 = CARTESIAN_POINT ( 'NONE',  ( 3.621962727011649896, 15.57349433917915427, -0.6543932647608998732 ) ) ;
#21357 = VERTEX_POINT ( 'NONE', #12444 ) ;
#21358 = ITEM_DEFINED_TRANSFORMATION ( 'NONE', 'NONE', #16548,  #2234 ) ;
#21359 = FACE_OUTER_BOUND ( 'NONE', #13113, .T. ) ;
#21360 = CARTESIAN_POINT ( 'NONE',  ( 6.632063100419781421, 19.53589599333302118, 6.336315105421093996 ) ) ;
#21361 = DIRECTION ( 'NONE',  ( 0.000000000000000000, 1.000000000000000000, 0.000000000000000000 ) ) ;
#21362 = ORIENTED_EDGE ( 'NONE', *, *, #16309, .T. ) ;
#21363 = CIRCLE ( 'NONE', #4777, 0.5079999999999997851 ) ;
#21364 = CARTESIAN_POINT ( 'NONE',  ( 6.688107640665243103, 20.11689778289562014, 0.06817244078631719273 ) ) ;
#21365 = CARTESIAN_POINT ( 'NONE',  ( 5.155436405379945519, 17.75259917515757024, 7.809584811493537337 ) ) ;
#21366 = CARTESIAN_POINT ( 'NONE',  ( 4.884574842566780539, 11.05839472165502180, 3.726956720474497775 ) ) ;
#21367 = DIRECTION ( 'NONE',  ( -0.8609107660235850723, 0.000000000000000000, 0.5087559856598092844 ) ) ;
#21368 = DIRECTION ( 'NONE',  ( 0.000000000000000000, 1.000000000000000000, 0.000000000000000000 ) ) ;
#21369 = CARTESIAN_POINT ( 'NONE',  ( 6.767924793147533258, 11.30044898972404965, 2.706056956047799389 ) ) ;
#21370 = CARTESIAN_POINT ( 'NONE',  ( 28.97711086133420366, 0.000000000000000000, -10.31874999999999964 ) ) ;
#21371 = ADVANCED_FACE ( 'NONE', ( #19383 ), #10668, .F. ) ;
#21372 = CARTESIAN_POINT ( 'NONE',  ( 20.51158336189590869, -5.799430522514935404, -15.12126906808022575 ) ) ;
#21373 = CARTESIAN_POINT ( 'NONE',  ( -17.46249999999999858, 33.73373999999999739, 0.000000000000000000 ) ) ;
#21374 = ORIENTED_EDGE ( 'NONE', *, *, #8671, .T. ) ;
#21375 = DIRECTION ( 'NONE',  ( 0.000000000000000000, 1.000000000000000000, 0.000000000000000000 ) ) ;
#21376 = LINE ( 'NONE', #12895, #1998 ) ;
#21377 = VECTOR ( 'NONE', #9655, 1000.000000000000000 ) ;
#21378 = ORIENTED_EDGE ( 'NONE', *, *, #7960, .T. ) ;
#21379 = ADVANCED_FACE ( 'NONE', ( #17417 ), #9098, .F. ) ;
#21380 = CARTESIAN_POINT ( 'NONE',  ( 12.46412619058443738, 19.82591093859932485, 5.041212240312027859 ) ) ;
#21381 = DIRECTION ( 'NONE',  ( 0.000000000000000000, 1.000000000000000000, 0.000000000000000000 ) ) ;
#21382 = CARTESIAN_POINT ( 'NONE',  ( 0.7218944351460162556, 19.40741025969103362, 7.447597755446342838 ) ) ;
#21383 = EDGE_CURVE ( 'NONE', #14268, #8439, #6449, .T. ) ;
#21384 = CARTESIAN_POINT ( 'NONE',  ( 11.59212630941054023, -6.991794502677832313, -15.67875784842310338 ) ) ;
#21385 = CARTESIAN_POINT ( 'NONE',  ( -28.19602381335591801, 39.45064500000000152, -72.46697370030818774 ) ) ;
#21386 = VERTEX_POINT ( 'NONE', #8885 ) ;
#21387 = DIRECTION ( 'NONE',  ( 0.000000000000000000, 1.000000000000000000, 0.000000000000000000 ) ) ;
#21388 = CARTESIAN_POINT ( 'NONE',  ( 36.54633153140315471, -14.84248999999999974, -9.516661413425623550 ) ) ;
#21389 = ORIENTED_EDGE ( 'NONE', *, *, #8285, .T. ) ;
#21390 = CARTESIAN_POINT ( 'NONE',  ( 19.45582853530259371, 0.02454099089219423033, -15.02042049756312281 ) ) ;
#21391 = CARTESIAN_POINT ( 'NONE',  ( 0.6626195881407476174, 19.22990431264859623, 1.911452493813652120 ) ) ;
#21392 = CARTESIAN_POINT ( 'NONE',  ( 17.28264852343957969, 1.821796179831712603, -15.76246644883694614 ) ) ;
#21393 = VERTEX_POINT ( 'NONE', #2259 ) ;
#21394 = CARTESIAN_POINT ( 'NONE',  ( 11.10629993265927951, 14.44082934938793272, -3.329231321055425852 ) ) ;
#21395 = CARTESIAN_POINT ( 'NONE',  ( 38.57934937226391270, 39.92799049660965238, -4.392330771018444047 ) ) ;
#21396 = CARTESIAN_POINT ( 'NONE',  ( 7.705021094126213832, 11.34324505471928113, -0.1215938047098856639 ) ) ;
#21397 = ADVANCED_FACE ( 'NONE', ( #601 ), #14111, .F. ) ;
#21398 = CARTESIAN_POINT ( 'NONE',  ( 19.42743112357013757, -5.337970718820712612, -15.39200997442386409 ) ) ;
#21399 = SURFACE_STYLE_FILL_AREA ( #2956 ) ;
#21400 = ORIENTED_EDGE ( 'NONE', *, *, #20020, .F. ) ;
#21401 = FACE_OUTER_BOUND ( 'NONE', #6681, .T. ) ;
#21402 = LINE ( 'NONE', #13029, #1451 ) ;
#21403 = ORIENTED_EDGE ( 'NONE', *, *, #6553, .F. ) ;
#21404 = ORIENTED_EDGE ( 'NONE', *, *, #12684, .F. ) ;
#21405 = CARTESIAN_POINT ( 'NONE',  ( 14.57357923071240791, -8.662971838486674514, -15.12377395242994282 ) ) ;
#21406 = ADVANCED_FACE ( 'NONE', ( #5800 ), #7672, .T. ) ;
#21408 = LINE ( 'NONE', #7928, #3927 ) ;
#21407 = CARTESIAN_POINT ( 'NONE',  ( 0.1240714093338939339, 19.02512202735066182, 0.6848216044496894250 ) ) ;
#21409 = ORIENTED_EDGE ( 'NONE', *, *, #1701, .F. ) ;
#21410 = CARTESIAN_POINT ( 'NONE',  ( 3.563401380057076739, 13.90534388967183688, -0.8314790740504168776 ) ) ;
#21411 = ORIENTED_EDGE ( 'NONE', *, *, #6799, .F. ) ;
#21412 = EDGE_LOOP ( 'NONE', ( #16566, #15239, #14716, #5727 ) ) ;
#21413 = AXIS2_PLACEMENT_3D ( 'NONE', #8102, #19507, #9549 ) ;
#21414 = VERTEX_POINT ( 'NONE', #9209 ) ;
#21415 = CARTESIAN_POINT ( 'NONE',  ( 2.398074235537467125, 12.22537918657540246, 3.074432563163722154 ) ) ;
#21416 = DIRECTION ( 'NONE',  ( -0.3482992169606098365, 0.9330960544336215357, -0.08955115110948595747 ) ) ;
#21417 = EDGE_CURVE ( 'NONE', #6460, #19865, #15992, .T. ) ;
#21418 = FACE_OUTER_BOUND ( 'NONE', #5119, .T. ) ;
#21419 = CARTESIAN_POINT ( 'NONE',  ( 23.63592995296846766, 9.340595522457139310, -3.311609719350443015 ) ) ;
#21420 = DIRECTION ( 'NONE',  ( 0.000000000000000000, 1.000000000000000000, 0.000000000000000000 ) ) ;
#21421 = CARTESIAN_POINT ( 'NONE',  ( 2.443280369300999233, 11.34257332251352146, 3.338292367401025640 ) ) ;
#21422 = EDGE_CURVE ( 'NONE', #10146, #19201, #3977, .T. ) ;
#21423 = EDGE_CURVE ( 'NONE', #21532, #2434, #2923, .T. ) ;
#21424 = EDGE_LOOP ( 'NONE', ( #6638, #3159, #8630, #2301, #17450, #4838, #4127, #1633, #1855, #17533, #4297, #16782, #3807, #21743, #16666, #17563, #15918, #919, #16915, #13967, #5155, #14852 ) ) ;
#21425 = CARTESIAN_POINT ( 'NONE',  ( 38.60701496492545459, -1.983739999999999837, -26.94161103631838472 ) ) ;
#21426 = FACE_OUTER_BOUND ( 'NONE', #20638, .T. ) ;
#21427 = DIRECTION ( 'NONE',  ( -0.2868778675745011220, 0.000000000000000000, -0.9579671649362034858 ) ) ;
#21428 = FACE_OUTER_BOUND ( 'NONE', #8082, .T. ) ;
#21429 = EDGE_LOOP ( 'NONE', ( #11990, #948, #15056, #10894 ) ) ;
#21430 = EDGE_LOOP ( 'NONE', ( #15780, #4086, #6723, #17150, #828 ) ) ;
#21431 = CARTESIAN_POINT ( 'NONE',  ( 10.49070738783592915, 19.16255833366876260, 6.254498413846182103 ) ) ;
#21432 = VECTOR ( 'NONE', #1847, 1000.000000000000000 ) ;
#21433 = DIRECTION ( 'NONE',  ( 0.05085730733808393328, 0.000000000000000000, -0.9987059298363656357 ) ) ;
#21434 = CARTESIAN_POINT ( 'NONE',  ( 10.95919977160705905, 14.02423986086742680, -3.881915835329841080 ) ) ;
#21435 = ORIENTED_EDGE ( 'NONE', *, *, #4379, .F. ) ;
#21436 = ORIENTED_EDGE ( 'NONE', *, *, #19349, .F. ) ;
#21437 = LINE ( 'NONE', #10154, #9546 ) ;
#21438 = CARTESIAN_POINT ( 'NONE',  ( 7.971212282706394703, 20.65571312975535889, 4.348524338217387708 ) ) ;
#21439 = VECTOR ( 'NONE', #4069, 1000.000000000000000 ) ;
#21440 = CARTESIAN_POINT ( 'NONE',  ( -15.41509608936259035, 37.15413452960619622, -10.31276839742836415 ) ) ;
#21441 = DIRECTION ( 'NONE',  ( 0.000000000000000000, 1.000000000000000000, 0.000000000000000000 ) ) ;
#21442 = CYLINDRICAL_SURFACE ( 'NONE', #12005, 1.587500000000000577 ) ;
#21443 = DIRECTION ( 'NONE',  ( 0.2490110332224850509, 0.000000000000000000, -0.9685006480810792739 ) ) ;
#21444 = CARTESIAN_POINT ( 'NONE',  ( 1.351768079374881415, 12.22725232455871058, 7.465297556611946383 ) ) ;
#21445 = EDGE_CURVE ( 'NONE', #6011, #18301, #4688, .T. ) ;
#21446 = DIRECTION ( 'NONE',  ( 0.000000000000000000, 1.000000000000000000, 0.000000000000000000 ) ) ;
#21447 = ORIENTED_EDGE ( 'NONE', *, *, #15817, .F. ) ;
#21448 = CARTESIAN_POINT ( 'NONE',  ( 3.693332233841136514, 15.57283695825947412, -0.6801890634934508739 ) ) ;
#21449 = CYLINDRICAL_SURFACE ( 'NONE', #8820, 0.7950200000000005041 ) ;
#21450 = CARTESIAN_POINT ( 'NONE',  ( 53.90573468513591138, -6.034543792452756072, -15.68687799581064013 ) ) ;
#21451 = CARTESIAN_POINT ( 'NONE',  ( 14.22686132395239156, -8.224742894641035917, -15.24862271894013865 ) ) ;
#21452 = DIRECTION ( 'NONE',  ( 0.7532174416907910786, 0.000000000000000000, 0.6577716059034319773 ) ) ;
#21453 = ORIENTED_EDGE ( 'NONE', *, *, #6648, .T. ) ;
#21454 = CARTESIAN_POINT ( 'NONE',  ( 29.64606458365116737, 30.55334249999999940, -15.53894806404596096 ) ) ;
#21455 = CARTESIAN_POINT ( 'NONE',  ( 5.947658929124695071, 11.10665485570860156, 1.375830819723275145 ) ) ;
#21456 = ORIENTED_EDGE ( 'NONE', *, *, #6683, .T. ) ;
#21457 = CARTESIAN_POINT ( 'NONE',  ( 28.48640205779059897, 1.520289674025695037, 10.66088537228617916 ) ) ;
#21458 = CARTESIAN_POINT ( 'NONE',  ( 12.87278157376591992, 21.37109313374715214, 0.5016493235560532948 ) ) ;
#21459 = AXIS2_PLACEMENT_3D ( 'NONE', #16980, #65, #18857 ) ;
#21460 = CARTESIAN_POINT ( 'NONE',  ( 6.957760857039438918, 21.53600301301377229, 1.616326073237095651 ) ) ;
#21461 = DIRECTION ( 'NONE',  ( 0.4987171968201974948, 0.000000000000000000, -0.8667647648559582141 ) ) ;
#21462 = CARTESIAN_POINT ( 'NONE',  ( 0.8306377868003163023, 19.66973114709098169, 2.255943557795851984 ) ) ;
#21463 = SURFACE_STYLE_FILL_AREA ( #14757 ) ;
#21464 = SHAPE_REPRESENTATION ( 'Ratchet Main Fixed Frame', ( #2234 ), #16895 ) ;
#21465 = AXIS2_PLACEMENT_3D ( 'NONE', #1481, #11984, #15431 ) ;
#21466 = DIRECTION ( 'NONE',  ( 0.000000000000000000, 1.000000000000000000, 0.000000000000000000 ) ) ;
#21467 = CARTESIAN_POINT ( 'NONE',  ( 6.406648404943450004, 11.79079236785502260, 1.495512976961110185 ) ) ;
#21468 = CARTESIAN_POINT ( 'NONE',  ( 5.367040623886392581, 15.74799863055303284, 8.000260316783158743 ) ) ;
#21469 = DIRECTION ( 'NONE',  ( -1.000000000000000000, 0.000000000000000000, 0.000000000000000000 ) ) ;
#21470 = CARTESIAN_POINT ( 'NONE',  ( 4.109322517731720303, 12.26666322754141980, 0.3490965934614432831 ) ) ;
#21471 = CARTESIAN_POINT ( 'NONE',  ( 4.520836821130160388, 40.07707250000000698, -5.476444653012091379 ) ) ;
#21472 = EDGE_CURVE ( 'NONE', #11803, #10917, #6003, .T. ) ;
#21473 = DIRECTION ( 'NONE',  ( -0.9790635044817342925, 0.000000000000000000, 0.2035550397114870846 ) ) ;
#21474 = CARTESIAN_POINT ( 'NONE',  ( 6.600193629736931022, 11.65214223036289276, 2.781968066501882664 ) ) ;
#21475 = CARTESIAN_POINT ( 'NONE',  ( 39.80203592816771874, 39.51271241376007737, -3.118117012970574198 ) ) ;
#21476 = CARTESIAN_POINT ( 'NONE',  ( 20.11748764637184905, -6.374101614863125320, -15.19701450337229076 ) ) ;
#21477 = DIRECTION ( 'NONE',  ( -0.9943660382494290406, 0.000000000000000000, 0.1060008583745199739 ) ) ;
#21478 = ORIENTED_EDGE ( 'NONE', *, *, #6927, .F. ) ;
#21479 = LINE ( 'NONE', #17964, #14588 ) ;
#21480 = DIRECTION ( 'NONE',  ( 0.3542738219355897056, 0.000000000000000000, 0.9351417320872542627 ) ) ;
#21481 = EDGE_CURVE ( 'NONE', #8950, #21616, #21263, .T. ) ;
#21482 = VERTEX_POINT ( 'NONE', #4797 ) ;
#21483 = EDGE_CURVE ( 'NONE', #10146, #18443, #9432, .T. ) ;
#21484 = CARTESIAN_POINT ( 'NONE',  ( 10.67700820321931765, 20.99839770658254068, 0.2808976642710648286 ) ) ;
#21485 = CARTESIAN_POINT ( 'NONE',  ( 44.28293121686854761, -1.983739999999999393, -31.08068102505560759 ) ) ;
#21486 = CARTESIAN_POINT ( 'NONE',  ( 52.86882968722888876, 37.72141639867590612, -16.95806507629960791 ) ) ;
#21487 = CARTESIAN_POINT ( 'NONE',  ( 14.01160604672443100, 1.694280624689696868, -15.36152992422168317 ) ) ;
#21488 = CARTESIAN_POINT ( 'NONE',  ( 47.80475250345343596, 42.06303499999999929, -11.91473563638196786 ) ) ;
#21489 = VERTEX_POINT ( 'NONE', #1251 ) ;
#21490 = CARTESIAN_POINT ( 'NONE',  ( 8.011380105705496746, 24.59767750000000319, -19.05252355006962617 ) ) ;
#21491 = B_SPLINE_CURVE_WITH_KNOTS ( 'NONE', 3,
 ( #6398, #13277, #16368, #20085, #1529, #13167, #19876, #3089, #1207, #16583, #4951, #7950, #4637, #1419, #14940, #18128, #14721, #11706 ),
 .UNSPECIFIED., .F., .F.,
 ( 4, 2, 2, 2, 2, 2, 2, 2, 4 ),
 ( 0.000000000000000000, 0.0004692937272967107249, 0.0009385874545934214499, 0.001407881181890132229, 0.001877174909186842900, 0.002346468636483553787, 0.002815762363780264458, 0.003285056091076975129, 0.003754349818373685799 ),
 .UNSPECIFIED. ) ;
#21492 = CARTESIAN_POINT ( 'NONE',  ( 53.46798503507454825, -1.983739999999999837, 6.304111036318381878 ) ) ;
#21493 = VECTOR ( 'NONE', #13596, 1000.000000000000114 ) ;
#21494 = ORIENTED_EDGE ( 'NONE', *, *, #17921, .F. ) ;
#21495 = CARTESIAN_POINT ( 'NONE',  ( -2.256261688646920227, 22.62314500000000095, -0.3933872460174320240 ) ) ;
#21496 = PRODUCT_DEFINITION_SHAPE ( 'NONE', 'NONE',  #20592 ) ;
#21497 = CARTESIAN_POINT ( 'NONE',  ( 12.24295241119947519, -6.551777560806527845, -16.33579826273126301 ) ) ;
#21498 = ORIENTED_EDGE ( 'NONE', *, *, #1644, .T. ) ;
#21499 = FACE_OUTER_BOUND ( 'NONE', #883, .T. ) ;
#21500 = VECTOR ( 'NONE', #19692, 1000.000000000000227 ) ;
#21501 = DIRECTION ( 'NONE',  ( 0.000000000000000000, -1.000000000000000000, 0.000000000000000000 ) ) ;
#21502 = CARTESIAN_POINT ( 'NONE',  ( 5.641984309594026747, 12.08210925389420076, -0.3035586006813633664 ) ) ;
#21503 = EDGE_CURVE ( 'NONE', #2212, #5739, #16204, .T. ) ;
#21504 = EDGE_CURVE ( 'NONE', #2030, #3173, #7991, .T. ) ;
#21505 = CARTESIAN_POINT ( 'NONE',  ( 19.10695511661582202, -5.767362265322653947, -15.44912671492631517 ) ) ;
#21506 = CARTESIAN_POINT ( 'NONE',  ( 43.49132289107146931, -1.983739999999999837, 4.686923926377883021 ) ) ;
#21507 = ORIENTED_EDGE ( 'NONE', *, *, #15860, .T. ) ;
#21508 = CYLINDRICAL_SURFACE ( 'NONE', #2596, 0.7950200000000000600 ) ;
#21509 = DIRECTION ( 'NONE',  ( -0.5222415575336509797, 0.000000000000000000, -0.8527976052879290281 ) ) ;
#21510 = ORIENTED_EDGE ( 'NONE', *, *, #19050, .T. ) ;
#21511 = ORIENTED_EDGE ( 'NONE', *, *, #17122, .F. ) ;
#21512 = CIRCLE ( 'NONE', #3510, 25.00312500000000426 ) ;
#21513 = CARTESIAN_POINT ( 'NONE',  ( 70.64340948846358970, 32.54502000000000095, -10.93409647675949969 ) ) ;
#21515 = DIRECTION ( 'NONE',  ( -0.7421532822901579785, 0.000000000000000000, 0.6702301885068628895 ) ) ;
#21514 = CARTESIAN_POINT ( 'NONE',  ( 1.795691274907587509, 18.25402966388874049, -0.4402665253856706817 ) ) ;
#21516 = EDGE_LOOP ( 'NONE', ( #12155, #8704, #8934, #2419 ) ) ;
#21517 = CARTESIAN_POINT ( 'NONE',  ( 3.582146072703705997, 13.71129357845431684, -0.7217611990671898292 ) ) ;
#21518 = VECTOR ( 'NONE', #18061, 1000.000000000000000 ) ;
#21519 = ORIENTED_EDGE ( 'NONE', *, *, #2449, .T. ) ;
#21520 = VERTEX_POINT ( 'NONE', #18063 ) ;
#21521 = ADVANCED_FACE ( 'NONE', ( #2804 ), #14765, .F. ) ;
#21522 = CARTESIAN_POINT ( 'NONE',  ( 0.6793796526421052029, 12.22740754112877148, 4.469871391076155831 ) ) ;
#21523 = ORIENTED_EDGE ( 'NONE', *, *, #13066, .T. ) ;
#21524 = ADVANCED_FACE ( 'NONE', ( #11529 ), #12994, .F. ) ;
#21525 = EDGE_CURVE ( 'NONE', #8118, #10568, #14432, .T. ) ;
#21526 = VECTOR ( 'NONE', #12964, 1000.000000000000114 ) ;
#21527 = LINE ( 'NONE', #13156, #54 ) ;
#21528 = MECHANICAL_DESIGN_GEOMETRIC_PRESENTATION_REPRESENTATION (  '', ( #20112 ), #9877 ) ;
#21529 = DIRECTION ( 'NONE',  ( 0.9579671649362033747, 0.000000000000000000, -0.2868778675745011220 ) ) ;
#21530 = DIRECTION ( 'NONE',  ( -0.000000000000000000, -1.000000000000000000, 0.000000000000000000 ) ) ;
#21531 = CARTESIAN_POINT ( 'NONE',  ( 1.657803152234513355, 15.27370134203824925, -0.5790142783057288245 ) ) ;
#21532 = VERTEX_POINT ( 'NONE', #6328 ) ;
#21533 = CARTESIAN_POINT ( 'NONE',  ( 28.56548256563643662, 34.52875999999999834, -12.12873025803960658 ) ) ;
#21534 = DIRECTION ( 'NONE',  ( 0.000000000000000000, 1.000000000000000000, 0.000000000000000000 ) ) ;
#21535 = DIRECTION ( 'NONE',  ( 0.000000000000000000, 1.000000000000000000, 0.000000000000000000 ) ) ;
#21536 = CYLINDRICAL_SURFACE ( 'NONE', #10189, 25.00312499999999361 ) ;
#21537 = EDGE_CURVE ( 'NONE', #6939, #16850, #21644, .T. ) ;
#21538 = ORIENTED_EDGE ( 'NONE', *, *, #7682, .T. ) ;
#21539 = ORIENTED_EDGE ( 'NONE', *, *, #4646, .T. ) ;
#21540 = CARTESIAN_POINT ( 'NONE',  ( 13.12251614003352707, 21.80725978669622123, 2.472223153733141832 ) ) ;
#21541 = AXIS2_PLACEMENT_3D ( 'NONE', #19127, #3997, #13629 ) ;
#21542 = LINE ( 'NONE', #19987, #8021 ) ;
#21543 = CARTESIAN_POINT ( 'NONE',  ( 11.57882746174914601, 20.16567382252436857, -3.032094887718085996 ) ) ;
#21544 = EDGE_LOOP ( 'NONE', ( #21519, #10359 ) ) ;
#21545 = ORIENTED_EDGE ( 'NONE', *, *, #17796, .F. ) ;
#21546 = DIRECTION ( 'NONE',  ( -0.9999999999672709583, 8.090614674031770259E-06, -1.618640899075949903E-09 ) ) ;
#21547 = VECTOR ( 'NONE', #15192, 1000.000000000000114 ) ;
#21548 = EDGE_CURVE ( 'NONE', #16568, #14728, #4574, .T. ) ;
#21549 = CARTESIAN_POINT ( 'NONE',  ( 9.049540828476574816, 12.76716365958394661, 5.677328593145490210 ) ) ;
#21550 = CARTESIAN_POINT ( 'NONE',  ( 7.040843878398417743, 12.58136646072892262, 5.765943884753188087 ) ) ;
#21551 = EDGE_CURVE ( 'NONE', #19210, #7476, #13530, .T. ) ;
#21552 = ADVANCED_FACE ( 'NONE', ( #21587 ), #19813, .F. ) ;
#21553 = CARTESIAN_POINT ( 'NONE',  ( 3.216025952483349659, 17.66257927194542887, 8.239042406146007025 ) ) ;
#21554 = DIRECTION ( 'NONE',  ( -9.174536502825477718E-16, 1.000000000000000000, -1.085629106648973872E-14 ) ) ;
#21555 = VECTOR ( 'NONE', #19990, 1000.000000000000114 ) ;
#21556 = CIRCLE ( 'NONE', #4280, 9.524999999999996803 ) ;
#21557 = CARTESIAN_POINT ( 'NONE',  ( 53.14266576735298031, -7.546379553159687781, -16.66242751532464084 ) ) ;
#21558 = CYLINDRICAL_SURFACE ( 'NONE', #5982, 0.5080000000000001181 ) ;
#21559 = CARTESIAN_POINT ( 'NONE',  ( 5.125831596548154678, 19.21458830873230283, 8.081027414488584526 ) ) ;
#21560 = CARTESIAN_POINT ( 'NONE',  ( 1.687027707696350021, 14.46428959965339089, 9.250708045227060694 ) ) ;
#21561 = DIRECTION ( 'NONE',  ( 0.2868778675745011220, 0.000000000000000000, 0.9579671649362034858 ) ) ;
#21562 = ORIENTED_EDGE ( 'NONE', *, *, #14486, .F. ) ;
#21563 = CARTESIAN_POINT ( 'NONE',  ( 4.090297026962545601, 18.69411302701743338, -0.1436813144736139303 ) ) ;
#21564 = FACE_OUTER_BOUND ( 'NONE', #1865, .T. ) ;
#21565 = CARTESIAN_POINT ( 'NONE',  ( 20.55406668138206427, -5.109279823642991936, -13.90851210264134075 ) ) ;
#21566 = AXIS2_PLACEMENT_3D ( 'NONE', #21373, #15093, #11534 ) ;
#21567 = CARTESIAN_POINT ( 'NONE',  ( 2.063750000000000195, 30.16440499999999858, 8.731249999999999289 ) ) ;
#21568 = VERTEX_POINT ( 'NONE', #4361 ) ;
#21569 = CARTESIAN_POINT ( 'NONE',  ( 8.330980629002562310, 21.35551480289056059, -0.1344304400260789845 ) ) ;
#21570 = CARTESIAN_POINT ( 'NONE',  ( 9.314696995175902217, 18.34482884134195046, -3.294293335070737516 ) ) ;
#21571 = ORIENTED_EDGE ( 'NONE', *, *, #12516, .F. ) ;
#21572 = CIRCLE ( 'NONE', #18742, 0.7950200000000003930 ) ;
#21573 = CARTESIAN_POINT ( 'NONE',  ( 8.596786337317182003, 20.54162763964906446, 6.075574452332789477 ) ) ;
#21574 = DIRECTION ( 'NONE',  ( 0.000000000000000000, 1.000000000000000000, 0.000000000000000000 ) ) ;
#21575 = CARTESIAN_POINT ( 'NONE',  ( 6.917740723153603000, 12.34712571434790007, 5.616724432863675176 ) ) ;
#21576 = VECTOR ( 'NONE', #3261, 1000.000000000000000 ) ;
#21577 = EDGE_CURVE ( 'NONE', #12681, #14041, #6447, .T. ) ;
#21578 = CARTESIAN_POINT ( 'NONE',  ( 30.42699695299585017, 34.52875999999999834, -4.832012189960551041 ) ) ;
#21579 = ADVANCED_FACE ( 'NONE', ( #11100 ), #9539, .T. ) ;
#21580 = PLANE ( 'NONE',  #15014 ) ;
#21581 = AXIS2_PLACEMENT_3D ( 'NONE', #21129, #5981, #2686 ) ;
#21582 = DIRECTION ( 'NONE',  ( 1.000000000000000000, 0.000000000000000000, 0.000000000000000000 ) ) ;
#21583 = CARTESIAN_POINT ( 'NONE',  ( 14.19715987342163466, 20.58788406416984174, 3.804178473946510763 ) ) ;
#21584 = AXIS2_PLACEMENT_3D ( 'NONE', #8982, #7332, #10429 ) ;
#21585 = CARTESIAN_POINT ( 'NONE',  ( 56.91751438644678984, 32.54502000000000095, -20.96198986413465448 ) ) ;
#21586 = CARTESIAN_POINT ( 'NONE',  ( 7.550821753472927611, 18.47894807998623534, 7.895890258472527456 ) ) ;
#21587 = FACE_OUTER_BOUND ( 'NONE', #21808, .T. ) ;
#21588 = CIRCLE ( 'NONE', #12067, 1.587500000000001688 ) ;
#21589 = AXIS2_PLACEMENT_3D ( 'NONE', #10403, #17148, #19122 ) ;
#21590 = DIRECTION ( 'NONE',  ( 0.000000000000000000, 1.000000000000000000, 0.000000000000000000 ) ) ;
#21591 = CARTESIAN_POINT ( 'NONE',  ( 61.60152099976809126, 34.52875999999999834, -12.48877542598203405 ) ) ;
#21592 = DIRECTION ( 'NONE',  ( -0.6702301885068639997, 0.000000000000000000, -0.7421532822901570903 ) ) ;
#21593 = CARTESIAN_POINT ( 'NONE',  ( 64.14292646034530776, -1.983739999999999837, -12.24881465648521939 ) ) ;
#21594 = CARTESIAN_POINT ( 'NONE',  ( 52.49113927203492125, -7.547609999999999708, -16.14695822742135078 ) ) ;
#21595 = AXIS2_PLACEMENT_3D ( 'NONE', #4523, #16365, #12947 ) ;
#21596 = EDGE_LOOP ( 'NONE', ( #4701, #4390, #16461, #7301 ) ) ;
#21597 = LINE ( 'NONE', #18382, #9979 ) ;
#21598 = DIRECTION ( 'NONE',  ( 0.000000000000000000, 1.000000000000000000, 0.000000000000000000 ) ) ;
#21599 = VERTEX_POINT ( 'NONE', #11431 ) ;
#21600 = CARTESIAN_POINT ( 'NONE',  ( 12.89029027226322732, 12.39999842064192670, 4.636274517891662228 ) ) ;
#21601 =( BOUNDED_CURVE ( )  B_SPLINE_CURVE ( 3, ( #7275, #11107, #17330, #17860 ),
 .UNSPECIFIED., .F., .T. ) 
 B_SPLINE_CURVE_WITH_KNOTS ( ( 4, 4 ),
 ( 1.199226304266461929, 1.570796326795209863 ),
 .UNSPECIFIED. ) 
 CURVE ( )  GEOMETRIC_REPRESENTATION_ITEM ( )  RATIONAL_B_SPLINE_CURVE ( ( 1.000000000000000000, 0.9885276984537190170, 0.9885276984537190170, 1.000000000000000000 ) ) 
 REPRESENTATION_ITEM ( '' )  );
#21602 = CARTESIAN_POINT ( 'NONE',  ( -3.037751992662818257, 2.373947500000000765, -30.02724401157551526 ) ) ;
#21603 = CARTESIAN_POINT ( 'NONE',  ( 12.22927362527537731, -5.743469473357618149, -16.38050967881292053 ) ) ;
#21605 = FACE_OUTER_BOUND ( 'NONE', #8616, .T. ) ;
#21604 = CARTESIAN_POINT ( 'NONE',  ( 5.501791265511759121, 11.93061510394686131, 0.9090210824104238974 ) ) ;
#21606 = ORIENTED_EDGE ( 'NONE', *, *, #4822, .T. ) ;
#21607 =( NAMED_UNIT ( * ) SI_UNIT ( $, .STERADIAN. ) SOLID_ANGLE_UNIT ( ) );
#21608 = CARTESIAN_POINT ( 'NONE',  ( 8.011380105705496746, 39.28205249999999893, -19.05252355006962617 ) ) ;
#21609 = CARTESIAN_POINT ( 'NONE',  ( 3.798728974633189814, 16.66492728325505013, -0.6608801330569669119 ) ) ;
#21610 = EDGE_CURVE ( 'NONE', #19979, #20985, #5045, .T. ) ;
#21611 = CARTESIAN_POINT ( 'NONE',  ( 11.82678039945931481, -3.968114999999999615, -12.74436900065013667 ) ) ;
#21612 = AXIS2_PLACEMENT_3D ( 'NONE', #9932, #9819, #15051 ) ;
#21613 = VERTEX_POINT ( 'NONE', #18587 ) ;
#21614 = CARTESIAN_POINT ( 'NONE',  ( -3.037751992662818257, 2.373947500000000765, -30.02724401157551526 ) ) ;
#21615 = CARTESIAN_POINT ( 'NONE',  ( 0.3256322356561986986, 18.10962087754353789, 1.158861095437264233 ) ) ;
#21616 = VERTEX_POINT ( 'NONE', #11635 ) ;
#21617 = B_SPLINE_CURVE_WITH_KNOTS ( 'NONE', 3,
 ( #6687, #11781, #1175, #3380, #18400, #18093, #18204, #16762, #1278, #3056, #7915, #13132, #8019, #14689, #21395, #6249, #9780, #11664 ),
 .UNSPECIFIED., .F., .F.,
 ( 4, 2, 2, 2, 2, 2, 2, 2, 4 ),
 ( 0.003754349818373638095, 0.004223755935673031287, 0.004693162052972424045, 0.005162568170271817670, 0.005631974287571210429, 0.006101380404870604054, 0.006570786522169996813, 0.007040192639469389571, 0.007509598756768783197 ),
 .UNSPECIFIED. ) ;
#21618 = CARTESIAN_POINT ( 'NONE',  ( 9.877816227279955896, 11.51518149844540240, 0.4592217285865553555 ) ) ;
#21619 = CARTESIAN_POINT ( 'NONE',  ( 1.532169971477637782, 5.548947500000001476, -20.71839214105750315 ) ) ;
#21620 = CARTESIAN_POINT ( 'NONE',  ( 9.037814056838087140, 11.49988781216720213, 5.512589366362954379 ) ) ;
#21621 = CARTESIAN_POINT ( 'NONE',  ( 14.46430160870318460, -6.938395347649755962, -16.39814615911750550 ) ) ;
#21622 = DIRECTION ( 'NONE',  ( 0.000000000000000000, 1.000000000000000000, 0.000000000000000000 ) ) ;
#21623 = ORIENTED_EDGE ( 'NONE', *, *, #21709, .T. ) ;
#21624 = CARTESIAN_POINT ( 'NONE',  ( 10.31240588659874291, 20.19701905685399623, 4.945787191147431372 ) ) ;
#21625 = CARTESIAN_POINT ( 'NONE',  ( 11.34884033191374364, 22.16525292274814163, 2.020784021226117666 ) ) ;
#21626 = CARTESIAN_POINT ( 'NONE',  ( 24.71252020198295085, 23.75961143032650114, -0.7333271064221494884 ) ) ;
#21627 = VERTEX_POINT ( 'NONE', #8211 ) ;
#21628 = ORIENTED_EDGE ( 'NONE', *, *, #17583, .T. ) ;
#21629 = CIRCLE ( 'NONE', #5379, 8.929687500000000000 ) ;
#21630 = CARTESIAN_POINT ( 'NONE',  ( 9.828862065001116477, -1.983739999999999393, -16.12522240043857025 ) ) ;
#21631 = VECTOR ( 'NONE', #12579, 1000.000000000000114 ) ;
#21633 = DIRECTION ( 'NONE',  ( -0.000000000000000000, -1.000000000000000000, 0.000000000000000000 ) ) ;
#21632 = CARTESIAN_POINT ( 'NONE',  ( 1.387196809356705973, 12.54098868903164110, 8.059042662999539530 ) ) ;
#21634 = ORIENTED_EDGE ( 'NONE', *, *, #12944, .F. ) ;
#21635 = CARTESIAN_POINT ( 'NONE',  ( 6.267479123942431229, 21.08335768476283434, 5.486273385999922425 ) ) ;
#21636 = VERTEX_POINT ( 'NONE', #3562 ) ;
#21637 = EDGE_CURVE ( 'NONE', #19617, #1298, #14967, .T. ) ;
#21638 = ORIENTED_EDGE ( 'NONE', *, *, #19401, .F. ) ;
#21639 = VECTOR ( 'NONE', #10041, 1000.000000000000114 ) ;
#21640 = FACE_OUTER_BOUND ( 'NONE', #3609, .T. ) ;
#21641 = ORIENTED_EDGE ( 'NONE', *, *, #2922, .T. ) ;
#21642 = CARTESIAN_POINT ( 'NONE',  ( 2.196290092118426518, 12.65458560452110248, 2.124815543687548214 ) ) ;
#21643 = CARTESIAN_POINT ( 'NONE',  ( 12.45174026680245838, 21.52809012965692403, -1.595795982066800400 ) ) ;
#21644 = CIRCLE ( 'NONE', #3643, 9.524999999999996803 ) ;
#21645 = CARTESIAN_POINT ( 'NONE',  ( -17.46249999999999858, 33.73373999999999739, 0.000000000000000000 ) ) ;
#21646 = DIRECTION ( 'NONE',  ( 0.2868778675745010664, 0.000000000000000000, 0.9579671649362032637 ) ) ;
#21647 = PLANE ( 'NONE',  #11478 ) ;
#21648 = CARTESIAN_POINT ( 'NONE',  ( 1.970306187853680280, 18.49127644496248735, -0.2525819039933897003 ) ) ;
#21649 = ORIENTED_EDGE ( 'NONE', *, *, #21637, .T. ) ;
#21650 = DIRECTION ( 'NONE',  ( 0.000000000000000000, 1.000000000000000000, 0.000000000000000000 ) ) ;
#21651 = DIRECTION ( 'NONE',  ( 0.3447671952293626108, 0.000000000000000000, 0.9386882235831439658 ) ) ;
#21652 = CARTESIAN_POINT ( 'NONE',  ( 13.27863086949880156, 21.38512400881313624, 1.870058080168869763 ) ) ;
#21653 = EDGE_CURVE ( 'NONE', #4933, #10689, #2221, .T. ) ;
#21654 = CARTESIAN_POINT ( 'NONE',  ( 46.03750000000000142, 0.000000000000000000, -10.31874999999999964 ) ) ;
#21655 = AXIS2_PLACEMENT_3D ( 'NONE', #17852, #2699, #9430 ) ;
#21656 = VERTEX_POINT ( 'NONE', #20236 ) ;
#21657 = ORIENTED_EDGE ( 'NONE', *, *, #8046, .T. ) ;
#21658 = CARTESIAN_POINT ( 'NONE',  ( 11.77575330418671307, 21.24843477279145887, -1.235931630819451899 ) ) ;
#21659 = LINE ( 'NONE', #16480, #4495 ) ;
#21660 = EDGE_LOOP ( 'NONE', ( #2476, #1611, #1606, #5251 ) ) ;
#21661 = ORIENTED_EDGE ( 'NONE', *, *, #13479, .T. ) ;
#21662 = LINE ( 'NONE', #16800, #8849 ) ;
#21663 = EDGE_CURVE ( 'NONE', #2434, #2822, #16831, .T. ) ;
#21664 = AXIS2_PLACEMENT_3D ( 'NONE', #15633, #15846, #14079 ) ;
#21665 = EDGE_CURVE ( 'NONE', #14041, #3111, #20125, .T. ) ;
#21666 = EDGE_CURVE ( 'NONE', #4834, #6050, #14256, .T. ) ;
#21667 = CARTESIAN_POINT ( 'NONE',  ( 8.934272239977493868, 12.32793309878939247, 5.125849249461625234 ) ) ;
#21668 = CIRCLE ( 'NONE', #15350, 0.3962400000000000366 ) ;
#21669 = DIRECTION ( 'NONE',  ( 0.000000000000000000, -1.000000000000000000, -0.000000000000000000 ) ) ;
#21670 = DIRECTION ( 'NONE',  ( 0.9790635044817341814, 0.000000000000000000, -0.2035550397114870014 ) ) ;
#21671 = CARTESIAN_POINT ( 'NONE',  ( -3.845402119898529758, 26.98019749999999917, -31.39393985263922460 ) ) ;
#21672 = CARTESIAN_POINT ( 'NONE',  ( -0.06146464470125744678, 17.35439399542458716, 0.1308547258846398387 ) ) ;
#21673 = DIRECTION ( 'NONE',  ( 0.08420877549337300871, 0.000000000000000000, 0.9964481331860212121 ) ) ;
#21674 = ORIENTED_EDGE ( 'NONE', *, *, #10925, .F. ) ;
#21675 = CARTESIAN_POINT ( 'NONE',  ( 1.398876202885256603, 20.32969464963275996, 3.494799452748480029 ) ) ;
#21676 = VECTOR ( 'NONE', #10391, 1000.000000000000227 ) ;
#21677 = DIRECTION ( 'NONE',  ( -0.6702301885068628895, 0.000000000000000000, -0.7421532822901579785 ) ) ;
#21678 = DIRECTION ( 'NONE',  ( -0.3697464814795228816, 0.9291326812858931028, 0.000000000000000000 ) ) ;
#21679 = CARTESIAN_POINT ( 'NONE',  ( 13.67756757867809725, 1.982787499999999481, 2.571257636385987144 ) ) ;
#21680 = EDGE_CURVE ( 'NONE', #5667, #13538, #12852, .T. ) ;
#21681 = EDGE_LOOP ( 'NONE', ( #18131, #14965, #18535, #166, #7516 ) ) ;
#21682 = PRODUCT_RELATED_PRODUCT_CATEGORY ( 'part', '', ( #4744 ) ) ;
#21683 = CARTESIAN_POINT ( 'NONE',  ( 13.27727761442571541, 16.76891278191635593, 7.308350614176763571 ) ) ;
#21684 = LINE ( 'NONE', #10070, #3954 ) ;
#21685 = CARTESIAN_POINT ( 'NONE',  ( 9.072002966528325274, 15.54209628577143221, -3.558562164394619476 ) ) ;
#21686 = ORIENTED_EDGE ( 'NONE', *, *, #2770, .T. ) ;
#21687 = AXIS2_PLACEMENT_3D ( 'NONE', #10778, #10671, #15880 ) ;
#21688 = EDGE_CURVE ( 'NONE', #14216, #7283, #20938, .T. ) ;
#21689 = CARTESIAN_POINT ( 'NONE',  ( 6.889273768381389829, 21.47949826730284428, 1.429458743405805032 ) ) ;
#21690 = CARTESIAN_POINT ( 'NONE',  ( 4.520836821130160388, 25.39269750000000059, -5.476444653012091379 ) ) ;
#21691 = CARTESIAN_POINT ( 'NONE',  ( 5.989966368381897333, 12.01572996145620209, 1.466525965593846292 ) ) ;
#21692 = EDGE_CURVE ( 'NONE', #831, #2705, #12125, .T. ) ;
#21693 = FACE_OUTER_BOUND ( 'NONE', #21516, .T. ) ;
#21694 = DIRECTION ( 'NONE',  ( 0.000000000000000000, 0.000000000000000000, 1.000000000000000000 ) ) ;
#21695 = CIRCLE ( 'NONE', #14304, 1.191259999999998209 ) ;
#21696 = CARTESIAN_POINT ( 'NONE',  ( 12.00508793966407595, 19.77353779035612291, -2.692760160476166398 ) ) ;
#21697 = CARTESIAN_POINT ( 'NONE',  ( 5.373035982240415898, 15.58686636370129897, 7.979283019396571142 ) ) ;
#21698 = VECTOR ( 'NONE', #760, 1000.000000000000000 ) ;
#21699 = CARTESIAN_POINT ( 'NONE',  ( -7.949728765565600597, -0.7997824999999986195, -34.47798802950714503 ) ) ;
#21700 = CARTESIAN_POINT ( 'NONE',  ( 2.208305404124148108, 18.21888756068997495, -0.4754449005480404500 ) ) ;
#21701 = CARTESIAN_POINT ( 'NONE',  ( -3.246390552019219999, 20.24316500000000119, 3.217431771123079987 ) ) ;
#21702 = CARTESIAN_POINT ( 'NONE',  ( 29.36887348155339694, 1.984374998761125219, 10.71562877576799977 ) ) ;
#21703 = CARTESIAN_POINT ( 'NONE',  ( 6.522247128157750318, 10.95050744324944247, 2.754069170700927938 ) ) ;
#21704 = CARTESIAN_POINT ( 'NONE',  ( 64.14292646034530776, 32.54502000000000095, -12.24881465648521939 ) ) ;
#21705 = CARTESIAN_POINT ( 'NONE',  ( 21.21167325040990903, -2.309581742399265281, -15.07358112151901963 ) ) ;
#21706 = EDGE_CURVE ( 'NONE', #16212, #9547, #2588, .T. ) ;
#21707 = EDGE_CURVE ( 'NONE', #18746, #13538, #18372, .T. ) ;
#21708 = CARTESIAN_POINT ( 'NONE',  ( 70.64340948846358970, 30.56064500000000095, -10.93409647675949969 ) ) ;
#21709 = EDGE_CURVE ( 'NONE', #17151, #21414, #15663, .T. ) ;
#21710 = ORIENTED_EDGE ( 'NONE', *, *, #419, .T. ) ;
#21711 = DIRECTION ( 'NONE',  ( 0.000000000000000000, -1.000000000000000000, -0.000000000000000000 ) ) ;
#21712 = FACE_OUTER_BOUND ( 'NONE', #1445, .T. ) ;
#21713 = CARTESIAN_POINT ( 'NONE',  ( 42.66304184606194383, -9.531985000000000596, -19.22597499813143784 ) ) ;
#21714 = CARTESIAN_POINT ( 'NONE',  ( 13.14439431963711513, 16.12856496372081239, 6.412664661205437433 ) ) ;
#21715 = CARTESIAN_POINT ( 'NONE',  ( 14.14084833952063747, 15.36419388438619649, -16.93566361603518899 ) ) ;
#21716 = CARTESIAN_POINT ( 'NONE',  ( -17.46249999999999858, 32.54247999999999763, 0.000000000000000000 ) ) ;
#21717 = CARTESIAN_POINT ( 'NONE',  ( 14.54316325888261119, -8.043841742527851224, -14.50243733777968380 ) ) ;
#21719 = DIRECTION ( 'NONE',  ( 0.08420877549337300871, 0.000000000000000000, 0.9964481331860212121 ) ) ;
#21718 = CARTESIAN_POINT ( 'NONE',  ( -0.2827414589499773756, 14.25064834509233158, 1.265090244379412532 ) ) ;
#21720 = ORIENTED_EDGE ( 'NONE', *, *, #9813, .T. ) ;
#21721 = VECTOR ( 'NONE', #18324, 1000.000000000000114 ) ;
#21722 = CARTESIAN_POINT ( 'NONE',  ( 61.03378281434940078, 34.52875999999999834, -11.91737544536021431 ) ) ;
#21723 = CARTESIAN_POINT ( 'NONE',  ( 27.93207353965470574, 34.52875999999999834, -8.388685343514779902 ) ) ;
#21724 = ORIENTED_EDGE ( 'NONE', *, *, #3867, .F. ) ;
#21725 = FACE_OUTER_BOUND ( 'NONE', #20058, .T. ) ;
#21726 = CARTESIAN_POINT ( 'NONE',  ( 11.62054768543827166, -3.675972292006682185, -16.17590813040945008 ) ) ;
#21727 = VERTEX_POINT ( 'NONE', #13750 ) ;
#21728 = CARTESIAN_POINT ( 'NONE',  ( 9.649387129231474347, 18.90675885874853890, -2.308582331309884328 ) ) ;
#21729 = LINE ( 'NONE', #6583, #9915 ) ;
#21730 = CARTESIAN_POINT ( 'NONE',  ( 12.23173370279073957, 21.60877823626870153, -1.575334389537728308 ) ) ;
#21731 = AXIS2_PLACEMENT_3D ( 'NONE', #13418, #5004, #16423 ) ;
#21732 = CARTESIAN_POINT ( 'NONE',  ( 14.82108974844347848, -7.069631093989277915, -16.32458675325787922 ) ) ;
#21733 = EDGE_CURVE ( 'NONE', #11228, #1298, #14986, .T. ) ;
#21734 = FACE_OUTER_BOUND ( 'NONE', #10147, .T. ) ;
#21735 = ORIENTED_EDGE ( 'NONE', *, *, #13717, .F. ) ;
#21736 = CARTESIAN_POINT ( 'NONE',  ( 10.22372860683003637, 20.36372907135105592, 4.717067546579229997 ) ) ;
#21737 = CARTESIAN_POINT ( 'NONE',  ( 10.45581712281804343, 21.01184353768176294, 5.351293286372672320 ) ) ;
#21738 = DIRECTION ( 'NONE',  ( 0.9980811434661737147, 0.000000000000000000, 0.06191955310929838502 ) ) ;
#21739 = VERTEX_POINT ( 'NONE', #3358 ) ;
#21740 = ORIENTED_EDGE ( 'NONE', *, *, #17069, .T. ) ;
#21741 = LINE ( 'NONE', #10227, #10567 ) ;
#21742 = CARTESIAN_POINT ( 'NONE',  ( 1.201291853872432203, 18.94469375348566231, 9.016395128387324931 ) ) ;
#21743 = ORIENTED_EDGE ( 'NONE', *, *, #14166, .T. ) ;
#21744 = CARTESIAN_POINT ( 'NONE',  ( 6.180567681604283159, 21.19261967444545292, 5.252651310456046829 ) ) ;
#21745 = VERTEX_POINT ( 'NONE', #130 ) ;
#21746 = ORIENTED_EDGE ( 'NONE', *, *, #7539, .T. ) ;
#21747 = FACE_BOUND ( 'NONE', #6046, .T. ) ;
#21748 = VERTEX_POINT ( 'NONE', #15188 ) ;
#21749 = CARTESIAN_POINT ( 'NONE',  ( 2.520634914125955195, 12.09468909812262716, 3.637039390294387164 ) ) ;
#21750 = CARTESIAN_POINT ( 'NONE',  ( 14.51673069786281900, 21.18286304486736427, 4.116190393922946278 ) ) ;
#21751 = DIRECTION ( 'NONE',  ( -0.6702301885068634446, 0.000000000000000000, -0.7421532822901576454 ) ) ;
#21752 = DIRECTION ( 'NONE',  ( 0.000000000000000000, 0.000000000000000000, -1.000000000000000000 ) ) ;
#21753 = CARTESIAN_POINT ( 'NONE',  ( 2.410440815022877992, 20.02928331742002754, 0.8004643519925526141 ) ) ;
#21754 = EDGE_CURVE ( 'NONE', #21107, #10001, #8917, .T. ) ;
#21755 = VERTEX_POINT ( 'NONE', #21800 ) ;
#21756 = DIRECTION ( 'NONE',  ( -0.5222415575336509797, 0.000000000000000000, -0.8527976052879290281 ) ) ;
#21757 = CARTESIAN_POINT ( 'NONE',  ( 30.78626241496060700, 30.50833916023545811, -2.552201779827368622 ) ) ;
#21758 = FACE_OUTER_BOUND ( 'NONE', #13761, .T. ) ;
#21759 = DIRECTION ( 'NONE',  ( 1.000000000000000000, 0.000000000000000000, 0.000000000000000000 ) ) ;
#21760 = EDGE_LOOP ( 'NONE', ( #8662, #17529, #14811, #11582 ) ) ;
#21761 = VERTEX_POINT ( 'NONE', #6556 ) ;
#21762 = CARTESIAN_POINT ( 'NONE',  ( 10.21327483022897376, 11.26810435610842198, 2.205732127587809455 ) ) ;
#21763 = CARTESIAN_POINT ( 'NONE',  ( 12.38912331111999343, -14.84248999999999974, 5.137219823516766759 ) ) ;
#21764 = ORIENTED_EDGE ( 'NONE', *, *, #8002, .T. ) ;
#21765 = EDGE_LOOP ( 'NONE', ( #13813, #3836, #14499, #17859, #17994 ) ) ;
#21766 = DIRECTION ( 'NONE',  ( 0.4987171968201974948, 0.000000000000000000, -0.8667647648559581031 ) ) ;
#21767 = VECTOR ( 'NONE', #141, 1000.000000000000000 ) ;
#21768 = ORIENTED_EDGE ( 'NONE', *, *, #16803, .F. ) ;
#21769 = CARTESIAN_POINT ( 'NONE',  ( 8.497508964807796161, 11.57115047926810369, 3.163812390448663248 ) ) ;
#21770 = CARTESIAN_POINT ( 'NONE',  ( 6.778338134665419012, 11.93678929795636101, 4.550199992997654874 ) ) ;
#21771 = CARTESIAN_POINT ( 'NONE',  ( 3.141658771633866643, 18.03423197346641160, 8.097196469975823874 ) ) ;
#21772 = DIRECTION ( 'NONE',  ( 0.000000000000000000, 1.000000000000000000, 0.000000000000000000 ) ) ;
#21773 = CARTESIAN_POINT ( 'NONE',  ( 13.62051399351888747, 17.23237496650334677, -17.80340391586448234 ) ) ;
#21774 = CARTESIAN_POINT ( 'NONE',  ( 39.27728671717661513, -1.983739999999999837, -23.95520057284206672 ) ) ;
#21775 = CARTESIAN_POINT ( 'NONE',  ( -0.1943992194620844105, 15.25965415824441074, 0.1619022894663725287 ) ) ;
#21776 = ADVANCED_FACE ( 'NONE', ( #3241 ), #9978, .T. ) ;
#21777 = CARTESIAN_POINT ( 'NONE',  ( -24.20935654380574320, 41.43438499999999891, -25.29247038871795894 ) ) ;
#21778 = AXIS2_PLACEMENT_3D ( 'NONE', #6458, #14553, #16428 ) ;
#21779 = EDGE_CURVE ( 'NONE', #13475, #17862, #11065, .T. ) ;
#21780 = ORIENTED_EDGE ( 'NONE', *, *, #4617, .F. ) ;
#21781 = CARTESIAN_POINT ( 'NONE',  ( 4.622599792338005997, 19.87391983916490190, 6.369022444568970265 ) ) ;
#21782 = CARTESIAN_POINT ( 'NONE',  ( 65.64431122251959039, 32.54502000000000095, -11.29787305743958115 ) ) ;
#21783 = DIRECTION ( 'NONE',  ( 0.000000000000000000, 1.000000000000000000, 0.000000000000000000 ) ) ;
#21784 = CARTESIAN_POINT ( 'NONE',  ( 25.66139003002496466, 2.770822500000000854, -0.04100069345253434805 ) ) ;
#21785 = DIRECTION ( 'NONE',  ( 0.000000000000000000, 1.000000000000000000, 0.000000000000000000 ) ) ;
#21786 = EDGE_LOOP ( 'NONE', ( #10905, #2632, #6948, #11138, #2961, #5928 ) ) ;
#21787 = CARTESIAN_POINT ( 'NONE',  ( 12.31748130508202088, 20.46142704777525978, 5.647513992273966110 ) ) ;
#21788 = CARTESIAN_POINT ( 'NONE',  ( 9.385176790940363389, 12.04513265762483698, -1.737864651385272907 ) ) ;
#21789 = EDGE_LOOP ( 'NONE', ( #4855, #642, #11644, #17445 ) ) ;
#21790 = CARTESIAN_POINT ( 'NONE',  ( 9.230190439779004663, 18.33056329402273832, 7.627282159427823949 ) ) ;
#21791 = DIRECTION ( 'NONE',  ( -0.2490110332224850231, 0.000000000000000000, 0.9685006480810791629 ) ) ;
#21792 = DIRECTION ( 'NONE',  ( 0.000000000000000000, -1.000000000000000000, -0.000000000000000000 ) ) ;
#21793 = DIRECTION ( 'NONE',  ( 0.000000000000000000, 0.000000000000000000, 1.000000000000000000 ) ) ;
#21794 = AXIS2_PLACEMENT_3D ( 'NONE', #12245, #8691, #7036 ) ;
#21795 = DIRECTION ( 'NONE',  ( 1.000000000000000000, 0.000000000000000000, 0.000000000000000000 ) ) ;
#21796 = EDGE_CURVE ( 'NONE', #6011, #19768, #13529, .T. ) ;
#21797 = CARTESIAN_POINT ( 'NONE',  ( 11.16053233441080828, 11.27323348914452161, 3.901379546146052757 ) ) ;
#21798 = CARTESIAN_POINT ( 'NONE',  ( -15.40073180542343501, -4.594366328436724878, -10.30507461945350833 ) ) ;
#21799 = CARTESIAN_POINT ( 'NONE',  ( 6.299708290859729054, 11.35334887747070276, 1.087827900068284670 ) ) ;
#21800 = CARTESIAN_POINT ( 'NONE',  ( -7.545238043312568088, -1.594802499999999013, -33.79351368943453338 ) ) ;
#21801 = EDGE_CURVE ( 'NONE', #18960, #1819, #12476, .T. ) ;
#21802 = DIRECTION ( 'NONE',  ( 0.000000000000000000, 0.000000000000000000, -1.000000000000000000 ) ) ;
#21803 = CARTESIAN_POINT ( 'NONE',  ( 2.423484750520774167, 19.25858774544496299, 1.029796980820462116 ) ) ;
#21804 = CARTESIAN_POINT ( 'NONE',  ( 29.36874999999999858, 22.62187499999999929, 10.71562499999999929 ) ) ;
#21805 = CARTESIAN_POINT ( 'NONE',  ( 15.81640869719298870, -8.433271052806768253, -16.11895057086533356 ) ) ;
#21806 =( NAMED_UNIT ( * ) PLANE_ANGLE_UNIT ( ) SI_UNIT ( $, .RADIAN. ) );
#21807 = CIRCLE ( 'NONE', #5205, 1.983740000000000059 ) ;
#21808 = EDGE_LOOP ( 'NONE', ( #19836, #2903, #13941, #1612 ) ) ;
#21809 = CARTESIAN_POINT ( 'NONE',  ( 17.22522857595987844, -1.983739999999999393, -15.04442098945225403 ) ) ;
#21810 = LINE ( 'NONE', #5121, #5177 ) ;
#21811 = EDGE_CURVE ( 'NONE', #8805, #10798, #10699, .T. ) ;
#21812 = ORIENTED_EDGE ( 'NONE', *, *, #16068, .F. ) ;
#21813 = CARTESIAN_POINT ( 'NONE',  ( 12.49260597456722266, 19.74893178700066443, 5.112473264219437041 ) ) ;
#21814 = DIRECTION ( 'NONE',  ( 0.000000000000000000, -1.000000000000000000, 0.000000000000000000 ) ) ;
#21815 = DIRECTION ( 'NONE',  ( -0.3482992169606098365, 0.9330960544336215357, -0.08955115110948595747 ) ) ;
#21816 = CARTESIAN_POINT ( 'NONE',  ( 12.42461531891860105, -5.659038248882215072, -16.66875675070026830 ) ) ;
#21818 = CARTESIAN_POINT ( 'NONE',  ( 42.35466991749225940, -1.983739999999999837, -17.94967221382040279 ) ) ;
#21817 = CARTESIAN_POINT ( 'NONE',  ( 1.233214924422777692, 13.15932452227622207, 7.544853154380925631 ) ) ;
#21819 = VERTEX_POINT ( 'NONE', #10852 ) ;
#21820 = DIRECTION ( 'NONE',  ( 0.000000000000000000, 0.000000000000000000, 1.000000000000000000 ) ) ;
#21821 = CARTESIAN_POINT ( 'NONE',  ( -29.36874999999999858, 30.16440499999999858, 8.731249999999999289 ) ) ;
#21822 = CARTESIAN_POINT ( 'NONE',  ( 4.135061152470012047, 18.65628895784566765, -0.06275338617684531051 ) ) ;
#21823 = CARTESIAN_POINT ( 'NONE',  ( 6.380166963026771221, 10.92343582149830183, 2.794643371853744007 ) ) ;
#21824 = EDGE_CURVE ( 'NONE', #8918, #18428, #19355, .T. ) ;
#21825 = EDGE_CURVE ( 'NONE', #11084, #11404, #20790, .T. ) ;
#21826 = ADVANCED_FACE ( 'NONE', ( #7322 ), #20569, .T. ) ;
#21827 = AXIS2_PLACEMENT_3D ( 'NONE', #10462, #18631, #10566 ) ;
#21828 = CARTESIAN_POINT ( 'NONE',  ( 14.20148524362829257, -8.473402551277725792, -16.61869953724475124 ) ) ;
#21829 = EDGE_LOOP ( 'NONE', ( #961, #14802, #11439, #8756, #15710, #10235 ) ) ;
#21830 = CARTESIAN_POINT ( 'NONE',  ( 10.99711771549974060, 12.61666159072338189, 5.348159617015018519 ) ) ;
#21831 = CARTESIAN_POINT ( 'NONE',  ( 8.643606387840399918, 19.62966740229102314, 6.039244586192593189 ) ) ;
#21832 = CARTESIAN_POINT ( 'NONE',  ( -21.29909891687151813, 42.13594019876639862, -25.53841317587618320 ) ) ;
#21833 = CARTESIAN_POINT ( 'NONE',  ( 9.008345345023000661, 15.28249587578532065, -3.627796638107509963 ) ) ;
#21834 = CARTESIAN_POINT ( 'NONE',  ( 12.06866590677377005, -4.286523879175909713, -16.83933591760442283 ) ) ;
#21835 = PRODUCT_DEFINITION_CONTEXT ( 'detailed design', #19766, 'design' ) ;
#21836 = FACE_OUTER_BOUND ( 'NONE', #5480, .T. ) ;
#21837 = EDGE_LOOP ( 'NONE', ( #2290, #15368, #20280, #4278 ) ) ;
#21838 = CARTESIAN_POINT ( 'NONE',  ( 9.957777320403202737, 20.74193055653752893, 4.019321122224012832 ) ) ;
#21839 = CARTESIAN_POINT ( 'NONE',  ( 7.579231183649110193, 21.81319771123894213, 3.241726534174046659 ) ) ;
#21840 = DIRECTION ( 'NONE',  ( -0.2490110332224850231, 0.000000000000000000, 0.9685006480810791629 ) ) ;
#21841 = ORIENTED_EDGE ( 'NONE', *, *, #12438, .F. ) ;
#21842 = EDGE_LOOP ( 'NONE', ( #6277, #12593, #13703, #19904 ) ) ;
#21843 = VECTOR ( 'NONE', #4665, 1000.000000000000114 ) ;
#21844 = CARTESIAN_POINT ( 'NONE',  ( 29.22749461619170219, 38.48766750000000059, -4.986088976786413163 ) ) ;
#21846 = DIRECTION ( 'NONE',  ( 1.000000000000000000, 0.000000000000000000, 0.000000000000000000 ) ) ;
#21845 = CARTESIAN_POINT ( 'NONE',  ( 3.982884606420732165, 21.32044071393296036, 5.285254693471478582 ) ) ;
#21847 = ORIENTED_EDGE ( 'NONE', *, *, #20309, .T. ) ;
#21848 = CARTESIAN_POINT ( 'NONE',  ( 7.220887966238155542, 18.59188200624751985, 7.907029918178476890 ) ) ;
#21849 = VERTEX_POINT ( 'NONE', #12297 ) ;
#21850 = AXIS2_PLACEMENT_3D ( 'NONE', #14533, #12761, #2692 ) ;
#21851 = EDGE_CURVE ( 'NONE', #16869, #18112, #7543, .T. ) ;
#21852 = CARTESIAN_POINT ( 'NONE',  ( 48.58367710892853353, 34.52875999999999834, -25.32442392637788231 ) ) ;
#21853 = ORIENTED_EDGE ( 'NONE', *, *, #3741, .T. ) ;
#21854 = CARTESIAN_POINT ( 'NONE',  ( 1.988580286269568953, 13.59073803854975182, 1.058507375892315805 ) ) ;
#21855 = CARTESIAN_POINT ( 'NONE',  ( 3.780609725159723045, 14.10045209010493750, -0.05903433680642554415 ) ) ;
#21856 = AXIS2_PLACEMENT_3D ( 'NONE', #5491, #10144, #18975 ) ;
#21857 = DIRECTION ( 'NONE',  ( -0.9037041334408600912, -0.3596272420165190775, -0.2323512126103423614 ) ) ;
#21858 = CARTESIAN_POINT ( 'NONE',  ( -51.02421882195815783, 38.25938500000000175, -23.02637480153789795 ) ) ;
#21859 = CARTESIAN_POINT ( 'NONE',  ( 1.673089330097931704, 15.97351425540567327, -0.6816346176204383100 ) ) ;
#21860 = AXIS2_PLACEMENT_3D ( 'NONE', #17667, #19635, #9248 ) ;
#21861 = ORIENTED_EDGE ( 'NONE', *, *, #20264, .T. ) ;
#21862 = DIRECTION ( 'NONE',  ( -0.9987059298363656357, 0.000000000000000000, -0.05085730733808393328 ) ) ;
#21863 = DIRECTION ( 'NONE',  ( 0.8334497143791951279, 0.000000000000000000, 0.5525953072558960066 ) ) ;
#21864 = DIRECTION ( 'NONE',  ( 0.000000000000000000, 1.000000000000000000, 0.000000000000000000 ) ) ;
#21865 = FACE_OUTER_BOUND ( 'NONE', #9283, .T. ) ;
#21866 = VECTOR ( 'NONE', #1572, 1000.000000000000114 ) ;
#21867 = CARTESIAN_POINT ( 'NONE',  ( -51.69815163306579819, -14.84248999999999974, -7.436124251198355850 ) ) ;
#21868 = VERTEX_POINT ( 'NONE', #19254 ) ;
#21869 = VERTEX_POINT ( 'NONE', #4113 ) ;
#21870 = CARTESIAN_POINT ( 'NONE',  ( 8.025198030962046758, 20.59028652745482191, 4.762507451596738051 ) ) ;
#21871 = CARTESIAN_POINT ( 'NONE',  ( 12.88040283537677588, 19.43893749999999798, -0.09070320285213756550 ) ) ;
#21872 = EDGE_LOOP ( 'NONE', ( #9609, #3072, #17917, #15021 ) ) ;
#21873 = ORIENTED_EDGE ( 'NONE', *, *, #4471, .F. ) ;
#21874 = DIRECTION ( 'NONE',  ( 0.000000000000000000, 1.000000000000000000, 0.000000000000000000 ) ) ;
#21875 = ORIENTED_EDGE ( 'NONE', *, *, #3771, .F. ) ;
#21876 = CARTESIAN_POINT ( 'NONE',  ( 9.270245272572291029, 14.90869586488222076, 7.012989310538706889 ) ) ;
#21877 = EDGE_CURVE ( 'NONE', #21636, #8219, #15400, .T. ) ;
#21878 = AXIS2_PLACEMENT_3D ( 'NONE', #8331, #18385, #9993 ) ;
#21879 = AXIS2_PLACEMENT_3D ( 'NONE', #8408, #20445, #15519 ) ;
#21880 = CARTESIAN_POINT ( 'NONE',  ( -7.545238043312568088, 34.12394749999999988, -33.79351368943453338 ) ) ;
#21881 = CYLINDRICAL_SURFACE ( 'NONE', #12552, 0.3962400000000008138 ) ;
#21882 = DIRECTION ( 'NONE',  ( 0.000000000000000000, -1.000000000000000000, 0.000000000000000000 ) ) ;
#21883 = NEXT_ASSEMBLY_USAGE_OCCURRENCE ( 'NAUO1', ' ', ' ', #18695, #471, $ ) ;
#21884 = NEXT_ASSEMBLY_USAGE_OCCURRENCE ( 'NAUO2', ' ', ' ', #18695, #11551, $ ) ;
#21885 = NEXT_ASSEMBLY_USAGE_OCCURRENCE ( 'NAUO3', ' ', ' ', #18695, #19378, $ ) ;
#21886 = NEXT_ASSEMBLY_USAGE_OCCURRENCE ( 'NAUO4', ' ', ' ', #18695, #3715, $ ) ;
#21887 = NEXT_ASSEMBLY_USAGE_OCCURRENCE ( 'NAUO5', ' ', ' ', #18695, #5596, $ ) ;
#21888 = NEXT_ASSEMBLY_USAGE_OCCURRENCE ( 'NAUO6', ' ', ' ', #18695, #17378, $ ) ;
#21889 = NEXT_ASSEMBLY_USAGE_OCCURRENCE ( 'NAUO7', ' ', ' ', #18695, #1012, $ ) ;
#21890 = NEXT_ASSEMBLY_USAGE_OCCURRENCE ( 'NAUO8', ' ', ' ', #18695, #20592, $ ) ;
ENDSEC;
END-ISO-10303-21;
